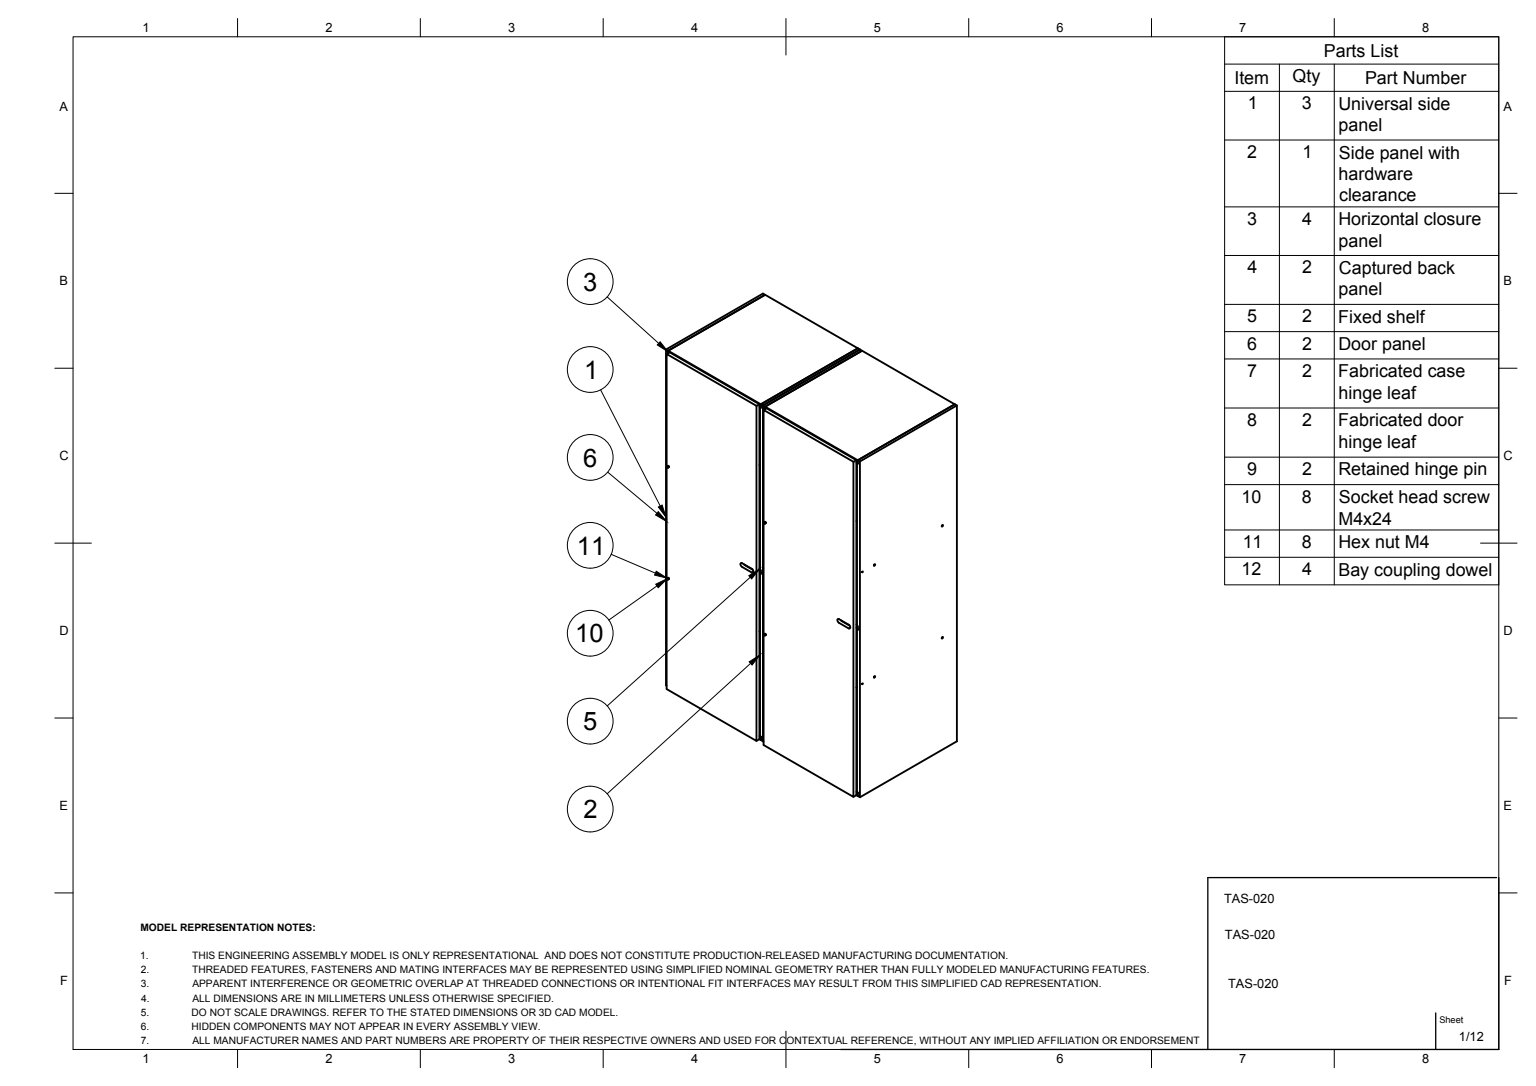
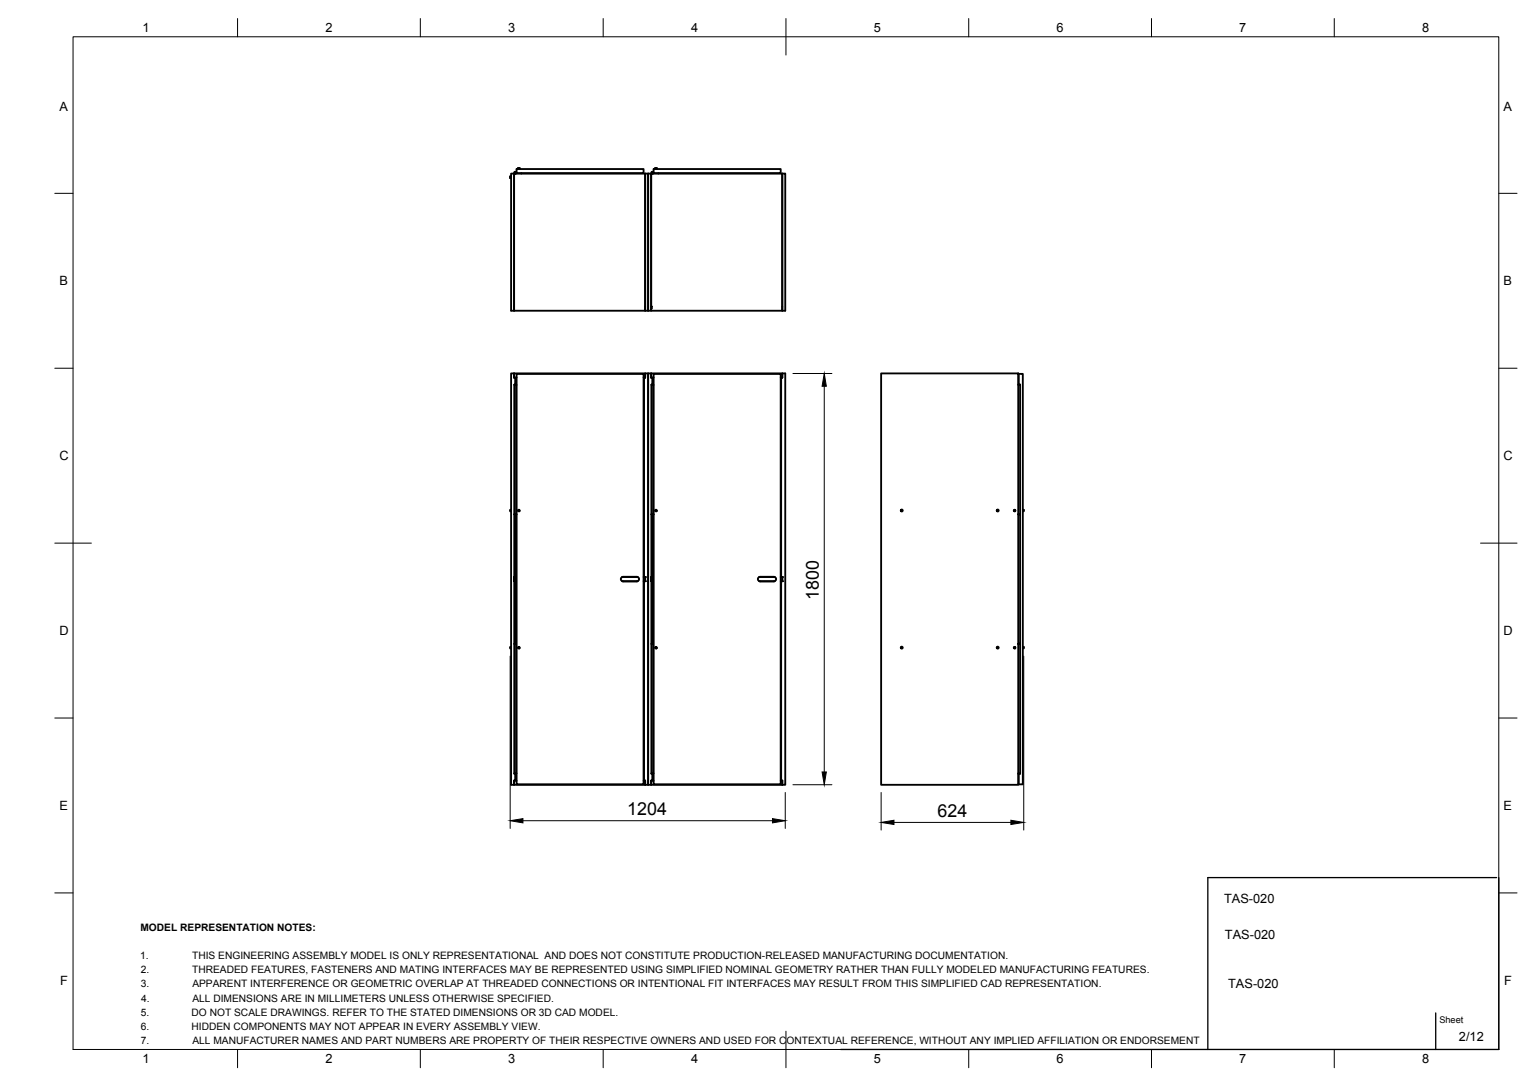
ISO-10303-21;
HEADER;
/* Generated by software containing ST-Developer
 * from STEP Tools, Inc. (www.steptools.com) 
 */

FILE_DESCRIPTION(
/* description */ (''),
/* implementation_level */ '2;1');

FILE_NAME(
/* name */ 'TAS-020.step',
/* time_stamp */ '2026-11-15T17:46:57-08:00',
/* author */ (''),
/* organization */ (''),
/* preprocessor_version */ 'ST-DEVELOPER v20.2',
/* originating_system */ 'Autodesk Translation Framework v15.17.0.0',
/* authorisation */ '');

FILE_SCHEMA (('AUTOMOTIVE_DESIGN { 1 0 10303 214 3 1 1 }'));
ENDSEC;

DATA;
#10=MECHANICAL_DESIGN_GEOMETRIC_PRESENTATION_REPRESENTATION('',(#375,#376,
#377,#378,#379,#380,#381,#382,#383,#384,#385,#386),#12963);
#11=ITEM_DEFINED_TRANSFORMATION($,$,#5008,#5301);
#12=ITEM_DEFINED_TRANSFORMATION($,$,#4955,#5302);
#13=ITEM_DEFINED_TRANSFORMATION($,$,#5053,#5303);
#14=ITEM_DEFINED_TRANSFORMATION($,$,#5064,#5304);
#15=ITEM_DEFINED_TRANSFORMATION($,$,#5071,#5305);
#16=ITEM_DEFINED_TRANSFORMATION($,$,#5080,#5306);
#17=ITEM_DEFINED_TRANSFORMATION($,$,#5101,#5307);
#18=ITEM_DEFINED_TRANSFORMATION($,$,#5134,#5308);
#19=ITEM_DEFINED_TRANSFORMATION($,$,#5163,#5309);
#20=ITEM_DEFINED_TRANSFORMATION($,$,#5177,#5310);
#21=ITEM_DEFINED_TRANSFORMATION($,$,#5267,#5311);
#22=ITEM_DEFINED_TRANSFORMATION($,$,#5295,#5312);
#23=ITEM_DEFINED_TRANSFORMATION($,$,#5053,#5313);
#24=ITEM_DEFINED_TRANSFORMATION($,$,#5177,#5314);
#25=ITEM_DEFINED_TRANSFORMATION($,$,#5267,#5315);
#26=ITEM_DEFINED_TRANSFORMATION($,$,#5177,#5316);
#27=ITEM_DEFINED_TRANSFORMATION($,$,#5267,#5317);
#28=ITEM_DEFINED_TRANSFORMATION($,$,#5177,#5318);
#29=ITEM_DEFINED_TRANSFORMATION($,$,#5267,#5319);
#30=ITEM_DEFINED_TRANSFORMATION($,$,#5008,#5320);
#31=ITEM_DEFINED_TRANSFORMATION($,$,#5008,#5321);
#32=ITEM_DEFINED_TRANSFORMATION($,$,#5053,#5322);
#33=ITEM_DEFINED_TRANSFORMATION($,$,#5053,#5323);
#34=ITEM_DEFINED_TRANSFORMATION($,$,#5064,#5324);
#35=ITEM_DEFINED_TRANSFORMATION($,$,#5071,#5325);
#36=ITEM_DEFINED_TRANSFORMATION($,$,#5080,#5326);
#37=ITEM_DEFINED_TRANSFORMATION($,$,#5101,#5327);
#38=ITEM_DEFINED_TRANSFORMATION($,$,#5134,#5328);
#39=ITEM_DEFINED_TRANSFORMATION($,$,#5163,#5329);
#40=ITEM_DEFINED_TRANSFORMATION($,$,#5177,#5330);
#41=ITEM_DEFINED_TRANSFORMATION($,$,#5267,#5331);
#42=ITEM_DEFINED_TRANSFORMATION($,$,#5177,#5332);
#43=ITEM_DEFINED_TRANSFORMATION($,$,#5267,#5333);
#44=ITEM_DEFINED_TRANSFORMATION($,$,#5177,#5334);
#45=ITEM_DEFINED_TRANSFORMATION($,$,#5267,#5335);
#46=ITEM_DEFINED_TRANSFORMATION($,$,#5177,#5336);
#47=ITEM_DEFINED_TRANSFORMATION($,$,#5267,#5337);
#48=ITEM_DEFINED_TRANSFORMATION($,$,#5295,#5338);
#49=ITEM_DEFINED_TRANSFORMATION($,$,#5295,#5339);
#50=ITEM_DEFINED_TRANSFORMATION($,$,#5295,#5340);
#51=(
REPRESENTATION_RELATIONSHIP($,$,#13036,#13034)
REPRESENTATION_RELATIONSHIP_WITH_TRANSFORMATION(#11)
SHAPE_REPRESENTATION_RELATIONSHIP()
);
#52=(
REPRESENTATION_RELATIONSHIP($,$,#13035,#13034)
REPRESENTATION_RELATIONSHIP_WITH_TRANSFORMATION(#12)
SHAPE_REPRESENTATION_RELATIONSHIP()
);
#53=(
REPRESENTATION_RELATIONSHIP($,$,#13037,#13034)
REPRESENTATION_RELATIONSHIP_WITH_TRANSFORMATION(#13)
SHAPE_REPRESENTATION_RELATIONSHIP()
);
#54=(
REPRESENTATION_RELATIONSHIP($,$,#13038,#13034)
REPRESENTATION_RELATIONSHIP_WITH_TRANSFORMATION(#14)
SHAPE_REPRESENTATION_RELATIONSHIP()
);
#55=(
REPRESENTATION_RELATIONSHIP($,$,#13039,#13034)
REPRESENTATION_RELATIONSHIP_WITH_TRANSFORMATION(#15)
SHAPE_REPRESENTATION_RELATIONSHIP()
);
#56=(
REPRESENTATION_RELATIONSHIP($,$,#13040,#13034)
REPRESENTATION_RELATIONSHIP_WITH_TRANSFORMATION(#16)
SHAPE_REPRESENTATION_RELATIONSHIP()
);
#57=(
REPRESENTATION_RELATIONSHIP($,$,#13041,#13034)
REPRESENTATION_RELATIONSHIP_WITH_TRANSFORMATION(#17)
SHAPE_REPRESENTATION_RELATIONSHIP()
);
#58=(
REPRESENTATION_RELATIONSHIP($,$,#13042,#13034)
REPRESENTATION_RELATIONSHIP_WITH_TRANSFORMATION(#18)
SHAPE_REPRESENTATION_RELATIONSHIP()
);
#59=(
REPRESENTATION_RELATIONSHIP($,$,#13043,#13034)
REPRESENTATION_RELATIONSHIP_WITH_TRANSFORMATION(#19)
SHAPE_REPRESENTATION_RELATIONSHIP()
);
#60=(
REPRESENTATION_RELATIONSHIP($,$,#13044,#13034)
REPRESENTATION_RELATIONSHIP_WITH_TRANSFORMATION(#20)
SHAPE_REPRESENTATION_RELATIONSHIP()
);
#61=(
REPRESENTATION_RELATIONSHIP($,$,#13045,#13034)
REPRESENTATION_RELATIONSHIP_WITH_TRANSFORMATION(#21)
SHAPE_REPRESENTATION_RELATIONSHIP()
);
#62=(
REPRESENTATION_RELATIONSHIP($,$,#13046,#13034)
REPRESENTATION_RELATIONSHIP_WITH_TRANSFORMATION(#22)
SHAPE_REPRESENTATION_RELATIONSHIP()
);
#63=(
REPRESENTATION_RELATIONSHIP($,$,#13037,#13034)
REPRESENTATION_RELATIONSHIP_WITH_TRANSFORMATION(#23)
SHAPE_REPRESENTATION_RELATIONSHIP()
);
#64=(
REPRESENTATION_RELATIONSHIP($,$,#13044,#13034)
REPRESENTATION_RELATIONSHIP_WITH_TRANSFORMATION(#24)
SHAPE_REPRESENTATION_RELATIONSHIP()
);
#65=(
REPRESENTATION_RELATIONSHIP($,$,#13045,#13034)
REPRESENTATION_RELATIONSHIP_WITH_TRANSFORMATION(#25)
SHAPE_REPRESENTATION_RELATIONSHIP()
);
#66=(
REPRESENTATION_RELATIONSHIP($,$,#13044,#13034)
REPRESENTATION_RELATIONSHIP_WITH_TRANSFORMATION(#26)
SHAPE_REPRESENTATION_RELATIONSHIP()
);
#67=(
REPRESENTATION_RELATIONSHIP($,$,#13045,#13034)
REPRESENTATION_RELATIONSHIP_WITH_TRANSFORMATION(#27)
SHAPE_REPRESENTATION_RELATIONSHIP()
);
#68=(
REPRESENTATION_RELATIONSHIP($,$,#13044,#13034)
REPRESENTATION_RELATIONSHIP_WITH_TRANSFORMATION(#28)
SHAPE_REPRESENTATION_RELATIONSHIP()
);
#69=(
REPRESENTATION_RELATIONSHIP($,$,#13045,#13034)
REPRESENTATION_RELATIONSHIP_WITH_TRANSFORMATION(#29)
SHAPE_REPRESENTATION_RELATIONSHIP()
);
#70=(
REPRESENTATION_RELATIONSHIP($,$,#13036,#13034)
REPRESENTATION_RELATIONSHIP_WITH_TRANSFORMATION(#30)
SHAPE_REPRESENTATION_RELATIONSHIP()
);
#71=(
REPRESENTATION_RELATIONSHIP($,$,#13036,#13034)
REPRESENTATION_RELATIONSHIP_WITH_TRANSFORMATION(#31)
SHAPE_REPRESENTATION_RELATIONSHIP()
);
#72=(
REPRESENTATION_RELATIONSHIP($,$,#13037,#13034)
REPRESENTATION_RELATIONSHIP_WITH_TRANSFORMATION(#32)
SHAPE_REPRESENTATION_RELATIONSHIP()
);
#73=(
REPRESENTATION_RELATIONSHIP($,$,#13037,#13034)
REPRESENTATION_RELATIONSHIP_WITH_TRANSFORMATION(#33)
SHAPE_REPRESENTATION_RELATIONSHIP()
);
#74=(
REPRESENTATION_RELATIONSHIP($,$,#13038,#13034)
REPRESENTATION_RELATIONSHIP_WITH_TRANSFORMATION(#34)
SHAPE_REPRESENTATION_RELATIONSHIP()
);
#75=(
REPRESENTATION_RELATIONSHIP($,$,#13039,#13034)
REPRESENTATION_RELATIONSHIP_WITH_TRANSFORMATION(#35)
SHAPE_REPRESENTATION_RELATIONSHIP()
);
#76=(
REPRESENTATION_RELATIONSHIP($,$,#13040,#13034)
REPRESENTATION_RELATIONSHIP_WITH_TRANSFORMATION(#36)
SHAPE_REPRESENTATION_RELATIONSHIP()
);
#77=(
REPRESENTATION_RELATIONSHIP($,$,#13041,#13034)
REPRESENTATION_RELATIONSHIP_WITH_TRANSFORMATION(#37)
SHAPE_REPRESENTATION_RELATIONSHIP()
);
#78=(
REPRESENTATION_RELATIONSHIP($,$,#13042,#13034)
REPRESENTATION_RELATIONSHIP_WITH_TRANSFORMATION(#38)
SHAPE_REPRESENTATION_RELATIONSHIP()
);
#79=(
REPRESENTATION_RELATIONSHIP($,$,#13043,#13034)
REPRESENTATION_RELATIONSHIP_WITH_TRANSFORMATION(#39)
SHAPE_REPRESENTATION_RELATIONSHIP()
);
#80=(
REPRESENTATION_RELATIONSHIP($,$,#13044,#13034)
REPRESENTATION_RELATIONSHIP_WITH_TRANSFORMATION(#40)
SHAPE_REPRESENTATION_RELATIONSHIP()
);
#81=(
REPRESENTATION_RELATIONSHIP($,$,#13045,#13034)
REPRESENTATION_RELATIONSHIP_WITH_TRANSFORMATION(#41)
SHAPE_REPRESENTATION_RELATIONSHIP()
);
#82=(
REPRESENTATION_RELATIONSHIP($,$,#13044,#13034)
REPRESENTATION_RELATIONSHIP_WITH_TRANSFORMATION(#42)
SHAPE_REPRESENTATION_RELATIONSHIP()
);
#83=(
REPRESENTATION_RELATIONSHIP($,$,#13045,#13034)
REPRESENTATION_RELATIONSHIP_WITH_TRANSFORMATION(#43)
SHAPE_REPRESENTATION_RELATIONSHIP()
);
#84=(
REPRESENTATION_RELATIONSHIP($,$,#13044,#13034)
REPRESENTATION_RELATIONSHIP_WITH_TRANSFORMATION(#44)
SHAPE_REPRESENTATION_RELATIONSHIP()
);
#85=(
REPRESENTATION_RELATIONSHIP($,$,#13045,#13034)
REPRESENTATION_RELATIONSHIP_WITH_TRANSFORMATION(#45)
SHAPE_REPRESENTATION_RELATIONSHIP()
);
#86=(
REPRESENTATION_RELATIONSHIP($,$,#13044,#13034)
REPRESENTATION_RELATIONSHIP_WITH_TRANSFORMATION(#46)
SHAPE_REPRESENTATION_RELATIONSHIP()
);
#87=(
REPRESENTATION_RELATIONSHIP($,$,#13045,#13034)
REPRESENTATION_RELATIONSHIP_WITH_TRANSFORMATION(#47)
SHAPE_REPRESENTATION_RELATIONSHIP()
);
#88=(
REPRESENTATION_RELATIONSHIP($,$,#13046,#13034)
REPRESENTATION_RELATIONSHIP_WITH_TRANSFORMATION(#48)
SHAPE_REPRESENTATION_RELATIONSHIP()
);
#89=(
REPRESENTATION_RELATIONSHIP($,$,#13046,#13034)
REPRESENTATION_RELATIONSHIP_WITH_TRANSFORMATION(#49)
SHAPE_REPRESENTATION_RELATIONSHIP()
);
#90=(
REPRESENTATION_RELATIONSHIP($,$,#13046,#13034)
REPRESENTATION_RELATIONSHIP_WITH_TRANSFORMATION(#50)
SHAPE_REPRESENTATION_RELATIONSHIP()
);
#91=CONTEXT_DEPENDENT_SHAPE_REPRESENTATION(#51,#12994);
#92=CONTEXT_DEPENDENT_SHAPE_REPRESENTATION(#52,#12995);
#93=CONTEXT_DEPENDENT_SHAPE_REPRESENTATION(#53,#12996);
#94=CONTEXT_DEPENDENT_SHAPE_REPRESENTATION(#54,#12997);
#95=CONTEXT_DEPENDENT_SHAPE_REPRESENTATION(#55,#12998);
#96=CONTEXT_DEPENDENT_SHAPE_REPRESENTATION(#56,#12999);
#97=CONTEXT_DEPENDENT_SHAPE_REPRESENTATION(#57,#13000);
#98=CONTEXT_DEPENDENT_SHAPE_REPRESENTATION(#58,#13001);
#99=CONTEXT_DEPENDENT_SHAPE_REPRESENTATION(#59,#13002);
#100=CONTEXT_DEPENDENT_SHAPE_REPRESENTATION(#60,#13003);
#101=CONTEXT_DEPENDENT_SHAPE_REPRESENTATION(#61,#13004);
#102=CONTEXT_DEPENDENT_SHAPE_REPRESENTATION(#62,#13005);
#103=CONTEXT_DEPENDENT_SHAPE_REPRESENTATION(#63,#13006);
#104=CONTEXT_DEPENDENT_SHAPE_REPRESENTATION(#64,#13007);
#105=CONTEXT_DEPENDENT_SHAPE_REPRESENTATION(#65,#13008);
#106=CONTEXT_DEPENDENT_SHAPE_REPRESENTATION(#66,#13009);
#107=CONTEXT_DEPENDENT_SHAPE_REPRESENTATION(#67,#13010);
#108=CONTEXT_DEPENDENT_SHAPE_REPRESENTATION(#68,#13011);
#109=CONTEXT_DEPENDENT_SHAPE_REPRESENTATION(#69,#13012);
#110=CONTEXT_DEPENDENT_SHAPE_REPRESENTATION(#70,#13013);
#111=CONTEXT_DEPENDENT_SHAPE_REPRESENTATION(#71,#13014);
#112=CONTEXT_DEPENDENT_SHAPE_REPRESENTATION(#72,#13015);
#113=CONTEXT_DEPENDENT_SHAPE_REPRESENTATION(#73,#13016);
#114=CONTEXT_DEPENDENT_SHAPE_REPRESENTATION(#74,#13017);
#115=CONTEXT_DEPENDENT_SHAPE_REPRESENTATION(#75,#13018);
#116=CONTEXT_DEPENDENT_SHAPE_REPRESENTATION(#76,#13019);
#117=CONTEXT_DEPENDENT_SHAPE_REPRESENTATION(#77,#13020);
#118=CONTEXT_DEPENDENT_SHAPE_REPRESENTATION(#78,#13021);
#119=CONTEXT_DEPENDENT_SHAPE_REPRESENTATION(#79,#13022);
#120=CONTEXT_DEPENDENT_SHAPE_REPRESENTATION(#80,#13023);
#121=CONTEXT_DEPENDENT_SHAPE_REPRESENTATION(#81,#13024);
#122=CONTEXT_DEPENDENT_SHAPE_REPRESENTATION(#82,#13025);
#123=CONTEXT_DEPENDENT_SHAPE_REPRESENTATION(#83,#13026);
#124=CONTEXT_DEPENDENT_SHAPE_REPRESENTATION(#84,#13027);
#125=CONTEXT_DEPENDENT_SHAPE_REPRESENTATION(#85,#13028);
#126=CONTEXT_DEPENDENT_SHAPE_REPRESENTATION(#86,#13029);
#127=CONTEXT_DEPENDENT_SHAPE_REPRESENTATION(#87,#13030);
#128=CONTEXT_DEPENDENT_SHAPE_REPRESENTATION(#88,#13031);
#129=CONTEXT_DEPENDENT_SHAPE_REPRESENTATION(#89,#13032);
#130=CONTEXT_DEPENDENT_SHAPE_REPRESENTATION(#90,#13033);
#131=NEXT_ASSEMBLY_USAGE_OCCURRENCE('Universal side panel:1',
'Universal side panel:1','Universal side panel:1',#13048,#13050,
'Universal side panel:1');
#132=NEXT_ASSEMBLY_USAGE_OCCURRENCE(
'Side panel with hardware clearance:1',
'Side panel with hardware clearance:1',
'Side panel with hardware clearance:1',#13048,#13049,
'Side panel with hardware clearance:1');
#133=NEXT_ASSEMBLY_USAGE_OCCURRENCE('Horizontal closure panel:1',
'Horizontal closure panel:1','Horizontal closure panel:1',#13048,#13051,
'Horizontal closure panel:1');
#134=NEXT_ASSEMBLY_USAGE_OCCURRENCE('Captured back panel:1',
'Captured back panel:1','Captured back panel:1',#13048,#13052,
'Captured back panel:1');
#135=NEXT_ASSEMBLY_USAGE_OCCURRENCE('Fixed shelf:1','Fixed shelf:1',
'Fixed shelf:1',#13048,#13053,'Fixed shelf:1');
#136=NEXT_ASSEMBLY_USAGE_OCCURRENCE('Door panel:1','Door panel:1',
'Door panel:1',#13048,#13054,'Door panel:1');
#137=NEXT_ASSEMBLY_USAGE_OCCURRENCE('Fabricated case hinge leaf:1',
'Fabricated case hinge leaf:1','Fabricated case hinge leaf:1',#13048,#13055,
'Fabricated case hinge leaf:1');
#138=NEXT_ASSEMBLY_USAGE_OCCURRENCE('Fabricated door hinge leaf:1',
'Fabricated door hinge leaf:1','Fabricated door hinge leaf:1',#13048,#13056,
'Fabricated door hinge leaf:1');
#139=NEXT_ASSEMBLY_USAGE_OCCURRENCE('Retained hinge pin:1',
'Retained hinge pin:1','Retained hinge pin:1',#13048,#13057,
'Retained hinge pin:1');
#140=NEXT_ASSEMBLY_USAGE_OCCURRENCE('Socket head screw M4x24:1',
'Socket head screw M4x24:1','Socket head screw M4x24:1',#13048,#13058,
'Socket head screw M4x24:1');
#141=NEXT_ASSEMBLY_USAGE_OCCURRENCE('Hex nut M4:1','Hex nut M4:1',
'Hex nut M4:1',#13048,#13059,'Hex nut M4:1');
#142=NEXT_ASSEMBLY_USAGE_OCCURRENCE('Bay coupling dowel:1',
'Bay coupling dowel:1','Bay coupling dowel:1',#13048,#13060,
'Bay coupling dowel:1');
#143=NEXT_ASSEMBLY_USAGE_OCCURRENCE('Horizontal closure panel:2',
'Horizontal closure panel:2','Horizontal closure panel:2',#13048,#13051,
'Horizontal closure panel:2');
#144=NEXT_ASSEMBLY_USAGE_OCCURRENCE('Socket head screw M4x24:2',
'Socket head screw M4x24:2','Socket head screw M4x24:2',#13048,#13058,
'Socket head screw M4x24:2');
#145=NEXT_ASSEMBLY_USAGE_OCCURRENCE('Hex nut M4:2','Hex nut M4:2',
'Hex nut M4:2',#13048,#13059,'Hex nut M4:2');
#146=NEXT_ASSEMBLY_USAGE_OCCURRENCE('Socket head screw M4x24:3',
'Socket head screw M4x24:3','Socket head screw M4x24:3',#13048,#13058,
'Socket head screw M4x24:3');
#147=NEXT_ASSEMBLY_USAGE_OCCURRENCE('Hex nut M4:3','Hex nut M4:3',
'Hex nut M4:3',#13048,#13059,'Hex nut M4:3');
#148=NEXT_ASSEMBLY_USAGE_OCCURRENCE('Socket head screw M4x24:4',
'Socket head screw M4x24:4','Socket head screw M4x24:4',#13048,#13058,
'Socket head screw M4x24:4');
#149=NEXT_ASSEMBLY_USAGE_OCCURRENCE('Hex nut M4:4','Hex nut M4:4',
'Hex nut M4:4',#13048,#13059,'Hex nut M4:4');
#150=NEXT_ASSEMBLY_USAGE_OCCURRENCE('Universal side panel:2',
'Universal side panel:2','Universal side panel:2',#13048,#13050,
'Universal side panel:2');
#151=NEXT_ASSEMBLY_USAGE_OCCURRENCE('Universal side panel:3',
'Universal side panel:3','Universal side panel:3',#13048,#13050,
'Universal side panel:3');
#152=NEXT_ASSEMBLY_USAGE_OCCURRENCE('Horizontal closure panel:3',
'Horizontal closure panel:3','Horizontal closure panel:3',#13048,#13051,
'Horizontal closure panel:3');
#153=NEXT_ASSEMBLY_USAGE_OCCURRENCE('Horizontal closure panel:4',
'Horizontal closure panel:4','Horizontal closure panel:4',#13048,#13051,
'Horizontal closure panel:4');
#154=NEXT_ASSEMBLY_USAGE_OCCURRENCE('Captured back panel:2',
'Captured back panel:2','Captured back panel:2',#13048,#13052,
'Captured back panel:2');
#155=NEXT_ASSEMBLY_USAGE_OCCURRENCE('Fixed shelf:2','Fixed shelf:2',
'Fixed shelf:2',#13048,#13053,'Fixed shelf:2');
#156=NEXT_ASSEMBLY_USAGE_OCCURRENCE('Door panel:2','Door panel:2',
'Door panel:2',#13048,#13054,'Door panel:2');
#157=NEXT_ASSEMBLY_USAGE_OCCURRENCE('Fabricated case hinge leaf:2',
'Fabricated case hinge leaf:2','Fabricated case hinge leaf:2',#13048,#13055,
'Fabricated case hinge leaf:2');
#158=NEXT_ASSEMBLY_USAGE_OCCURRENCE('Fabricated door hinge leaf:2',
'Fabricated door hinge leaf:2','Fabricated door hinge leaf:2',#13048,#13056,
'Fabricated door hinge leaf:2');
#159=NEXT_ASSEMBLY_USAGE_OCCURRENCE('Retained hinge pin:2',
'Retained hinge pin:2','Retained hinge pin:2',#13048,#13057,
'Retained hinge pin:2');
#160=NEXT_ASSEMBLY_USAGE_OCCURRENCE('Socket head screw M4x24:5',
'Socket head screw M4x24:5','Socket head screw M4x24:5',#13048,#13058,
'Socket head screw M4x24:5');
#161=NEXT_ASSEMBLY_USAGE_OCCURRENCE('Hex nut M4:5','Hex nut M4:5',
'Hex nut M4:5',#13048,#13059,'Hex nut M4:5');
#162=NEXT_ASSEMBLY_USAGE_OCCURRENCE('Socket head screw M4x24:6',
'Socket head screw M4x24:6','Socket head screw M4x24:6',#13048,#13058,
'Socket head screw M4x24:6');
#163=NEXT_ASSEMBLY_USAGE_OCCURRENCE('Hex nut M4:6','Hex nut M4:6',
'Hex nut M4:6',#13048,#13059,'Hex nut M4:6');
#164=NEXT_ASSEMBLY_USAGE_OCCURRENCE('Socket head screw M4x24:7',
'Socket head screw M4x24:7','Socket head screw M4x24:7',#13048,#13058,
'Socket head screw M4x24:7');
#165=NEXT_ASSEMBLY_USAGE_OCCURRENCE('Hex nut M4:7','Hex nut M4:7',
'Hex nut M4:7',#13048,#13059,'Hex nut M4:7');
#166=NEXT_ASSEMBLY_USAGE_OCCURRENCE('Socket head screw M4x24:8',
'Socket head screw M4x24:8','Socket head screw M4x24:8',#13048,#13058,
'Socket head screw M4x24:8');
#167=NEXT_ASSEMBLY_USAGE_OCCURRENCE('Hex nut M4:8','Hex nut M4:8',
'Hex nut M4:8',#13048,#13059,'Hex nut M4:8');
#168=NEXT_ASSEMBLY_USAGE_OCCURRENCE('Bay coupling dowel:2',
'Bay coupling dowel:2','Bay coupling dowel:2',#13048,#13060,
'Bay coupling dowel:2');
#169=NEXT_ASSEMBLY_USAGE_OCCURRENCE('Bay coupling dowel:3',
'Bay coupling dowel:3','Bay coupling dowel:3',#13048,#13060,
'Bay coupling dowel:3');
#170=NEXT_ASSEMBLY_USAGE_OCCURRENCE('Bay coupling dowel:4',
'Bay coupling dowel:4','Bay coupling dowel:4',#13048,#13060,
'Bay coupling dowel:4');
#171=B_SPLINE_SURFACE_WITH_KNOTS('',3,3,((#9802,#9803,#9804,#9805,#9806,
#9807,#9808,#9809,#9810,#9811,#9812,#9813,#9814,#9815,#9816,#9817,#9818,
#9819,#9820,#9821,#9822,#9823,#9824,#9825,#9826,#9827,#9828,#9829,#9830,
#9831,#9832,#9833,#9834,#9835,#9836,#9837,#9838,#9839,#9840,#9841,#9842,
#9843,#9844,#9845,#9846,#9847,#9848,#9849,#9850,#9851,#9852,#9853,#9854,
#9855,#9856,#9857,#9858,#9859,#9860,#9861,#9862,#9863,#9864,#9865,#9866,
#9867,#9868,#9869,#9870,#9871,#9872,#9873,#9874,#9875,#9876,#9877,#9878,
#9879,#9880,#9881,#9882,#9883,#9884,#9885,#9886,#9887,#9888,#9889,#9890,
#9891,#9892,#9893,#9894,#9895,#9896,#9897,#9898,#9899,#9900,#9901,#9902,
#9903,#9904,#9905,#9906,#9907,#9908,#9909,#9910,#9911,#9912,#9913,#9914,
#9915,#9916,#9917,#9918,#9919,#9920,#9921,#9922,#9923,#9924,#9925,#9926,
#9927,#9928,#9929,#9930,#9931,#9932,#9933,#9934,#9935,#9936,#9937,#9938,
#9939,#9940,#9941,#9942,#9943,#9944,#9945,#9946,#9947,#9948,#9949,#9950,
#9951,#9952,#9953,#9954,#9955,#9956,#9957,#9958,#9959,#9960,#9961,#9962,
#9963,#9964,#9965,#9966,#9967,#9968,#9969,#9970,#9971,#9972,#9973,#9974,
#9975,#9976,#9977,#9978,#9979,#9980,#9981,#9982,#9983,#9984,#9985,#9986,
#9987,#9988,#9989,#9990,#9991,#9992,#9993,#9994,#9995,#9996,#9997,#9998,
#9999,#10000,#10001,#10002,#10003,#10004,#10005,#10006,#10007,#10008,#10009,
#10010,#10011,#10012,#10013,#10014,#10015,#10016,#10017,#10018,#10019,#10020,
#10021,#10022),(#10023,#10024,#10025,#10026,#10027,#10028,#10029,#10030,
#10031,#10032,#10033,#10034,#10035,#10036,#10037,#10038,#10039,#10040,#10041,
#10042,#10043,#10044,#10045,#10046,#10047,#10048,#10049,#10050,#10051,#10052,
#10053,#10054,#10055,#10056,#10057,#10058,#10059,#10060,#10061,#10062,#10063,
#10064,#10065,#10066,#10067,#10068,#10069,#10070,#10071,#10072,#10073,#10074,
#10075,#10076,#10077,#10078,#10079,#10080,#10081,#10082,#10083,#10084,#10085,
#10086,#10087,#10088,#10089,#10090,#10091,#10092,#10093,#10094,#10095,#10096,
#10097,#10098,#10099,#10100,#10101,#10102,#10103,#10104,#10105,#10106,#10107,
#10108,#10109,#10110,#10111,#10112,#10113,#10114,#10115,#10116,#10117,#10118,
#10119,#10120,#10121,#10122,#10123,#10124,#10125,#10126,#10127,#10128,#10129,
#10130,#10131,#10132,#10133,#10134,#10135,#10136,#10137,#10138,#10139,#10140,
#10141,#10142,#10143,#10144,#10145,#10146,#10147,#10148,#10149,#10150,#10151,
#10152,#10153,#10154,#10155,#10156,#10157,#10158,#10159,#10160,#10161,#10162,
#10163,#10164,#10165,#10166,#10167,#10168,#10169,#10170,#10171,#10172,#10173,
#10174,#10175,#10176,#10177,#10178,#10179,#10180,#10181,#10182,#10183,#10184,
#10185,#10186,#10187,#10188,#10189,#10190,#10191,#10192,#10193,#10194,#10195,
#10196,#10197,#10198,#10199,#10200,#10201,#10202,#10203,#10204,#10205,#10206,
#10207,#10208,#10209,#10210,#10211,#10212,#10213,#10214,#10215,#10216,#10217,
#10218,#10219,#10220,#10221,#10222,#10223,#10224,#10225,#10226,#10227,#10228,
#10229,#10230,#10231,#10232,#10233,#10234,#10235,#10236,#10237,#10238,#10239,
#10240,#10241,#10242,#10243),(#10244,#10245,#10246,#10247,#10248,#10249,
#10250,#10251,#10252,#10253,#10254,#10255,#10256,#10257,#10258,#10259,#10260,
#10261,#10262,#10263,#10264,#10265,#10266,#10267,#10268,#10269,#10270,#10271,
#10272,#10273,#10274,#10275,#10276,#10277,#10278,#10279,#10280,#10281,#10282,
#10283,#10284,#10285,#10286,#10287,#10288,#10289,#10290,#10291,#10292,#10293,
#10294,#10295,#10296,#10297,#10298,#10299,#10300,#10301,#10302,#10303,#10304,
#10305,#10306,#10307,#10308,#10309,#10310,#10311,#10312,#10313,#10314,#10315,
#10316,#10317,#10318,#10319,#10320,#10321,#10322,#10323,#10324,#10325,#10326,
#10327,#10328,#10329,#10330,#10331,#10332,#10333,#10334,#10335,#10336,#10337,
#10338,#10339,#10340,#10341,#10342,#10343,#10344,#10345,#10346,#10347,#10348,
#10349,#10350,#10351,#10352,#10353,#10354,#10355,#10356,#10357,#10358,#10359,
#10360,#10361,#10362,#10363,#10364,#10365,#10366,#10367,#10368,#10369,#10370,
#10371,#10372,#10373,#10374,#10375,#10376,#10377,#10378,#10379,#10380,#10381,
#10382,#10383,#10384,#10385,#10386,#10387,#10388,#10389,#10390,#10391,#10392,
#10393,#10394,#10395,#10396,#10397,#10398,#10399,#10400,#10401,#10402,#10403,
#10404,#10405,#10406,#10407,#10408,#10409,#10410,#10411,#10412,#10413,#10414,
#10415,#10416,#10417,#10418,#10419,#10420,#10421,#10422,#10423,#10424,#10425,
#10426,#10427,#10428,#10429,#10430,#10431,#10432,#10433,#10434,#10435,#10436,
#10437,#10438,#10439,#10440,#10441,#10442,#10443,#10444,#10445,#10446,#10447,
#10448,#10449,#10450,#10451,#10452,#10453,#10454,#10455,#10456,#10457,#10458,
#10459,#10460,#10461,#10462,#10463,#10464),(#10465,#10466,#10467,#10468,
#10469,#10470,#10471,#10472,#10473,#10474,#10475,#10476,#10477,#10478,#10479,
#10480,#10481,#10482,#10483,#10484,#10485,#10486,#10487,#10488,#10489,#10490,
#10491,#10492,#10493,#10494,#10495,#10496,#10497,#10498,#10499,#10500,#10501,
#10502,#10503,#10504,#10505,#10506,#10507,#10508,#10509,#10510,#10511,#10512,
#10513,#10514,#10515,#10516,#10517,#10518,#10519,#10520,#10521,#10522,#10523,
#10524,#10525,#10526,#10527,#10528,#10529,#10530,#10531,#10532,#10533,#10534,
#10535,#10536,#10537,#10538,#10539,#10540,#10541,#10542,#10543,#10544,#10545,
#10546,#10547,#10548,#10549,#10550,#10551,#10552,#10553,#10554,#10555,#10556,
#10557,#10558,#10559,#10560,#10561,#10562,#10563,#10564,#10565,#10566,#10567,
#10568,#10569,#10570,#10571,#10572,#10573,#10574,#10575,#10576,#10577,#10578,
#10579,#10580,#10581,#10582,#10583,#10584,#10585,#10586,#10587,#10588,#10589,
#10590,#10591,#10592,#10593,#10594,#10595,#10596,#10597,#10598,#10599,#10600,
#10601,#10602,#10603,#10604,#10605,#10606,#10607,#10608,#10609,#10610,#10611,
#10612,#10613,#10614,#10615,#10616,#10617,#10618,#10619,#10620,#10621,#10622,
#10623,#10624,#10625,#10626,#10627,#10628,#10629,#10630,#10631,#10632,#10633,
#10634,#10635,#10636,#10637,#10638,#10639,#10640,#10641,#10642,#10643,#10644,
#10645,#10646,#10647,#10648,#10649,#10650,#10651,#10652,#10653,#10654,#10655,
#10656,#10657,#10658,#10659,#10660,#10661,#10662,#10663,#10664,#10665,#10666,
#10667,#10668,#10669,#10670,#10671,#10672,#10673,#10674,#10675,#10676,#10677,
#10678,#10679,#10680,#10681,#10682,#10683,#10684,#10685)),.UNSPECIFIED.,
 .F.,.F.,.F.,(4,4),(4,1,1,1,1,1,1,1,1,1,1,1,1,1,1,1,1,1,1,1,1,1,1,1,1,1,
1,1,1,1,1,1,1,1,1,1,1,1,1,1,1,1,1,1,1,1,1,1,1,1,1,1,1,1,1,1,1,1,1,1,1,1,
1,1,1,1,1,1,1,1,1,1,1,1,1,1,1,1,1,1,1,1,1,1,1,1,1,1,1,1,1,1,1,1,1,1,1,1,
1,1,1,1,1,1,1,1,1,1,1,1,1,1,1,1,1,1,1,1,1,1,1,1,1,1,1,1,1,1,1,1,1,1,1,1,
1,1,1,1,1,1,1,1,1,1,1,1,1,1,1,1,1,1,1,1,1,1,1,1,1,1,1,1,1,1,1,1,1,1,1,1,
1,1,1,1,1,1,1,1,1,1,1,1,1,1,1,1,1,1,1,1,1,1,1,1,1,1,1,1,1,1,1,1,1,1,1,1,
1,1,1,1,1,1,1,1,1,1,1,1,4),(0.,0.0460148164544132),(8.31058692273996,9.30824121805847,
10.305895513377,11.3035498086955,12.301204104014,13.2988583993325,14.296512694651,
15.2941669899695,16.291821285288,17.2894755806066,18.2871298759251,19.2847841712436,
20.2824384665621,21.2800927618806,22.2777470571991,23.2754013525176,24.2730556478361,
25.2707099431546,26.2683642384732,27.2660185337917,28.2636728291102,29.2613271244287,
30.2589814197472,31.2566357150657,32.2542900103842,33.2519443057027,34.2495986010213,
35.2472528963398,36.2449071916583,37.2425614869768,38.2402157822953,39.2378700776138,
40.2355243729323,41.2331786682508,42.2308329635693,43.2284872588879,44.2261415542064,
45.2237958495249,46.2214501448434,47.2191044401619,48.2167587354804,49.2144130307989,
50.2120673261174,51.209721621436,52.2073759167545,53.205030212073,54.2026845073915,
55.20033880271,56.1979930980285,57.195647393347,58.1933016886655,59.190955983984,
60.1886102793026,61.1862645746211,62.1839188699396,63.1815731652581,64.1792274605766,
65.1768817558951,66.1745360512136,67.1721903465321,68.1698446418506,69.1674989371692,
70.1651532324877,71.1628075278062,72.1604618231247,73.1581161184432,74.1557704137617,
75.1534247090802,76.1510790043987,77.1487332997173,78.1463875950358,79.1440418903543,
80.1416961856728,81.1393504809913,82.1370047763098,83.1346590716283,84.1323133669468,
85.1299676622653,86.1276219575839,87.1252762529024,88.1229305482209,89.1205848435394,
90.1182391388579,91.1158934341764,92.1135477294949,93.1112020248134,94.1088563201319,
95.1065106154505,96.104164910769,97.1018192060875,98.099473501406,99.0971277967245,
100.094782092043,101.092436387362,102.09009068268,103.087744977999,104.085399273317,
105.083053568636,106.080707863954,107.078362159273,108.076016454591,109.07367074991,
110.071325045228,111.068979340547,112.066633635865,113.064287931184,114.061942226502,
115.059596521821,116.057250817139,117.054905112458,118.052559407776,119.050213703095,
120.047867998413,121.045522293732,122.04317658905,123.040830884369,124.038485179687,
125.036139475006,126.033793770324,127.031448065643,128.029102360961,129.02675665628,
130.024410951598,131.022065246917,132.019719542235,133.017373837554,134.015028132872,
135.012682428191,136.010336723509,137.007991018828,138.005645314146,139.003299609465,
140.000953904783,140.998608200102,141.99626249542,142.993916790739,143.991571086058,
144.989225381376,145.986879676695,146.984533972013,147.982188267332,148.97984256265,
149.977496857969,150.975151153287,151.972805448606,152.970459743924,153.968114039243,
154.965768334561,155.96342262988,156.961076925198,157.958731220517,158.956385515835,
159.954039811154,160.951694106472,161.949348401791,162.947002697109,163.944656992428,
164.942311287746,165.939965583065,166.937619878383,167.935274173702,168.93292846902,
169.930582764339,170.928237059657,171.925891354976,172.923545650294,173.921199945613,
174.918854240931,175.91650853625,176.914162831568,177.911817126887,178.909471422205,
179.907125717524,180.904780012842,181.902434308161,182.900088603479,183.897742898798,
184.895397194116,185.893051489435,186.890705784754,187.888360080072,188.886014375391,
189.883668670709,190.881322966028,191.878977261346,192.876631556665,193.874285851983,
194.871940147302,195.86959444262,196.867248737939,197.864903033257,198.862557328576,
199.860211623894,200.857865919213,201.855520214531,202.85317450985,203.850828805168,
204.848483100487,205.846137395805,206.843791691124,207.841445986442,208.839100281761,
209.836754577079,210.834408872398,211.832063167716,212.829717463035,213.827371758353,
214.825026053672,215.82268034899,216.820334644309,217.817988939627,218.815643234946,
219.813297530264,220.810951825583,221.808606120901,222.80626041622,223.803914711538,
224.801569006857,225.799223302175),.UNSPECIFIED.);
#172=B_SPLINE_SURFACE_WITH_KNOTS('',3,3,((#10819,#10820,#10821,#10822,#10823,
#10824,#10825,#10826,#10827,#10828,#10829,#10830,#10831,#10832,#10833,#10834,
#10835,#10836,#10837,#10838,#10839,#10840,#10841,#10842,#10843,#10844,#10845,
#10846,#10847,#10848,#10849,#10850,#10851,#10852,#10853,#10854,#10855,#10856,
#10857,#10858,#10859,#10860,#10861,#10862,#10863,#10864,#10865,#10866,#10867,
#10868,#10869,#10870,#10871,#10872,#10873,#10874,#10875,#10876,#10877,#10878,
#10879,#10880,#10881,#10882,#10883,#10884,#10885,#10886,#10887,#10888,#10889,
#10890,#10891,#10892,#10893,#10894,#10895,#10896,#10897,#10898,#10899,#10900,
#10901,#10902,#10903,#10904,#10905,#10906,#10907,#10908,#10909,#10910,#10911,
#10912,#10913,#10914,#10915,#10916,#10917,#10918,#10919,#10920,#10921,#10922,
#10923,#10924,#10925,#10926,#10927,#10928,#10929,#10930,#10931,#10932,#10933,
#10934,#10935,#10936,#10937,#10938,#10939,#10940,#10941,#10942,#10943,#10944,
#10945,#10946,#10947,#10948,#10949,#10950,#10951,#10952,#10953,#10954,#10955,
#10956,#10957,#10958,#10959,#10960,#10961,#10962,#10963,#10964,#10965,#10966,
#10967,#10968,#10969,#10970,#10971,#10972,#10973,#10974,#10975,#10976,#10977,
#10978,#10979,#10980,#10981,#10982,#10983,#10984,#10985,#10986,#10987,#10988,
#10989,#10990,#10991,#10992,#10993,#10994,#10995,#10996,#10997,#10998,#10999,
#11000,#11001,#11002,#11003,#11004,#11005,#11006,#11007,#11008,#11009,#11010,
#11011,#11012,#11013,#11014,#11015,#11016,#11017,#11018,#11019,#11020,#11021,
#11022,#11023,#11024,#11025,#11026,#11027,#11028,#11029,#11030,#11031,#11032,
#11033,#11034,#11035,#11036,#11037,#11038,#11039),(#11040,#11041,#11042,
#11043,#11044,#11045,#11046,#11047,#11048,#11049,#11050,#11051,#11052,#11053,
#11054,#11055,#11056,#11057,#11058,#11059,#11060,#11061,#11062,#11063,#11064,
#11065,#11066,#11067,#11068,#11069,#11070,#11071,#11072,#11073,#11074,#11075,
#11076,#11077,#11078,#11079,#11080,#11081,#11082,#11083,#11084,#11085,#11086,
#11087,#11088,#11089,#11090,#11091,#11092,#11093,#11094,#11095,#11096,#11097,
#11098,#11099,#11100,#11101,#11102,#11103,#11104,#11105,#11106,#11107,#11108,
#11109,#11110,#11111,#11112,#11113,#11114,#11115,#11116,#11117,#11118,#11119,
#11120,#11121,#11122,#11123,#11124,#11125,#11126,#11127,#11128,#11129,#11130,
#11131,#11132,#11133,#11134,#11135,#11136,#11137,#11138,#11139,#11140,#11141,
#11142,#11143,#11144,#11145,#11146,#11147,#11148,#11149,#11150,#11151,#11152,
#11153,#11154,#11155,#11156,#11157,#11158,#11159,#11160,#11161,#11162,#11163,
#11164,#11165,#11166,#11167,#11168,#11169,#11170,#11171,#11172,#11173,#11174,
#11175,#11176,#11177,#11178,#11179,#11180,#11181,#11182,#11183,#11184,#11185,
#11186,#11187,#11188,#11189,#11190,#11191,#11192,#11193,#11194,#11195,#11196,
#11197,#11198,#11199,#11200,#11201,#11202,#11203,#11204,#11205,#11206,#11207,
#11208,#11209,#11210,#11211,#11212,#11213,#11214,#11215,#11216,#11217,#11218,
#11219,#11220,#11221,#11222,#11223,#11224,#11225,#11226,#11227,#11228,#11229,
#11230,#11231,#11232,#11233,#11234,#11235,#11236,#11237,#11238,#11239,#11240,
#11241,#11242,#11243,#11244,#11245,#11246,#11247,#11248,#11249,#11250,#11251,
#11252,#11253,#11254,#11255,#11256,#11257,#11258,#11259,#11260),(#11261,
#11262,#11263,#11264,#11265,#11266,#11267,#11268,#11269,#11270,#11271,#11272,
#11273,#11274,#11275,#11276,#11277,#11278,#11279,#11280,#11281,#11282,#11283,
#11284,#11285,#11286,#11287,#11288,#11289,#11290,#11291,#11292,#11293,#11294,
#11295,#11296,#11297,#11298,#11299,#11300,#11301,#11302,#11303,#11304,#11305,
#11306,#11307,#11308,#11309,#11310,#11311,#11312,#11313,#11314,#11315,#11316,
#11317,#11318,#11319,#11320,#11321,#11322,#11323,#11324,#11325,#11326,#11327,
#11328,#11329,#11330,#11331,#11332,#11333,#11334,#11335,#11336,#11337,#11338,
#11339,#11340,#11341,#11342,#11343,#11344,#11345,#11346,#11347,#11348,#11349,
#11350,#11351,#11352,#11353,#11354,#11355,#11356,#11357,#11358,#11359,#11360,
#11361,#11362,#11363,#11364,#11365,#11366,#11367,#11368,#11369,#11370,#11371,
#11372,#11373,#11374,#11375,#11376,#11377,#11378,#11379,#11380,#11381,#11382,
#11383,#11384,#11385,#11386,#11387,#11388,#11389,#11390,#11391,#11392,#11393,
#11394,#11395,#11396,#11397,#11398,#11399,#11400,#11401,#11402,#11403,#11404,
#11405,#11406,#11407,#11408,#11409,#11410,#11411,#11412,#11413,#11414,#11415,
#11416,#11417,#11418,#11419,#11420,#11421,#11422,#11423,#11424,#11425,#11426,
#11427,#11428,#11429,#11430,#11431,#11432,#11433,#11434,#11435,#11436,#11437,
#11438,#11439,#11440,#11441,#11442,#11443,#11444,#11445,#11446,#11447,#11448,
#11449,#11450,#11451,#11452,#11453,#11454,#11455,#11456,#11457,#11458,#11459,
#11460,#11461,#11462,#11463,#11464,#11465,#11466,#11467,#11468,#11469,#11470,
#11471,#11472,#11473,#11474,#11475,#11476,#11477,#11478,#11479,#11480,#11481),
(#11482,#11483,#11484,#11485,#11486,#11487,#11488,#11489,#11490,#11491,
#11492,#11493,#11494,#11495,#11496,#11497,#11498,#11499,#11500,#11501,#11502,
#11503,#11504,#11505,#11506,#11507,#11508,#11509,#11510,#11511,#11512,#11513,
#11514,#11515,#11516,#11517,#11518,#11519,#11520,#11521,#11522,#11523,#11524,
#11525,#11526,#11527,#11528,#11529,#11530,#11531,#11532,#11533,#11534,#11535,
#11536,#11537,#11538,#11539,#11540,#11541,#11542,#11543,#11544,#11545,#11546,
#11547,#11548,#11549,#11550,#11551,#11552,#11553,#11554,#11555,#11556,#11557,
#11558,#11559,#11560,#11561,#11562,#11563,#11564,#11565,#11566,#11567,#11568,
#11569,#11570,#11571,#11572,#11573,#11574,#11575,#11576,#11577,#11578,#11579,
#11580,#11581,#11582,#11583,#11584,#11585,#11586,#11587,#11588,#11589,#11590,
#11591,#11592,#11593,#11594,#11595,#11596,#11597,#11598,#11599,#11600,#11601,
#11602,#11603,#11604,#11605,#11606,#11607,#11608,#11609,#11610,#11611,#11612,
#11613,#11614,#11615,#11616,#11617,#11618,#11619,#11620,#11621,#11622,#11623,
#11624,#11625,#11626,#11627,#11628,#11629,#11630,#11631,#11632,#11633,#11634,
#11635,#11636,#11637,#11638,#11639,#11640,#11641,#11642,#11643,#11644,#11645,
#11646,#11647,#11648,#11649,#11650,#11651,#11652,#11653,#11654,#11655,#11656,
#11657,#11658,#11659,#11660,#11661,#11662,#11663,#11664,#11665,#11666,#11667,
#11668,#11669,#11670,#11671,#11672,#11673,#11674,#11675,#11676,#11677,#11678,
#11679,#11680,#11681,#11682,#11683,#11684,#11685,#11686,#11687,#11688,#11689,
#11690,#11691,#11692,#11693,#11694,#11695,#11696,#11697,#11698,#11699,#11700,
#11701,#11702)),.UNSPECIFIED.,.F.,.F.,.F.,(4,4),(4,1,1,1,1,1,1,1,1,1,1,
1,1,1,1,1,1,1,1,1,1,1,1,1,1,1,1,1,1,1,1,1,1,1,1,1,1,1,1,1,1,1,1,1,1,1,1,
1,1,1,1,1,1,1,1,1,1,1,1,1,1,1,1,1,1,1,1,1,1,1,1,1,1,1,1,1,1,1,1,1,1,1,1,
1,1,1,1,1,1,1,1,1,1,1,1,1,1,1,1,1,1,1,1,1,1,1,1,1,1,1,1,1,1,1,1,1,1,1,1,
1,1,1,1,1,1,1,1,1,1,1,1,1,1,1,1,1,1,1,1,1,1,1,1,1,1,1,1,1,1,1,1,1,1,1,1,
1,1,1,1,1,1,1,1,1,1,1,1,1,1,1,1,1,1,1,1,1,1,1,1,1,1,1,1,1,1,1,1,1,1,1,1,
1,1,1,1,1,1,1,1,1,1,1,1,1,1,1,1,1,1,1,1,1,1,1,1,1,1,1,4),(0.,0.0460148164544132),
(11.6154215191109,12.6130758144294,13.6107301097479,14.6083844050664,15.6060387003849,
16.6036929957034,17.601347291022,18.5990015863405,19.596655881659,20.5943101769775,
21.591964472296,22.5896187676145,23.587273062933,24.5849273582515,25.58258165357,
26.5802359488886,27.5778902442071,28.5755445395256,29.5731988348441,30.5708531301626,
31.5685074254811,32.5661617207996,33.5638160161181,34.5614703114366,35.5591246067551,
36.5567789020737,37.5544331973922,38.5520874927107,39.5497417880292,40.5473960833477,
41.5450503786662,42.5427046739847,43.5403589693032,44.5380132646217,45.5356675599403,
46.5333218552588,47.5309761505773,48.5286304458958,49.5262847412143,50.5239390365328,
51.5215933318513,52.5192476271698,53.5169019224883,54.5145562178069,55.5122105131254,
56.5098648084439,57.5075191037624,58.5051733990809,59.5028276943994,60.5004819897179,
61.4981362850364,62.4957905803549,63.4934448756734,64.491099170992,65.4887534663105,
66.486407761629,67.4840620569475,68.481716352266,69.4793706475845,70.477024942903,
71.4746792382215,72.4723335335401,73.4699878288586,74.4676421241771,75.4652964194956,
76.4629507148141,77.4606050101326,78.4582593054511,79.4559136007696,80.4535678960881,
81.4512221914066,82.4488764867252,83.4465307820437,84.4441850773622,85.4418393726807,
86.4394936679992,87.4371479633177,88.4348022586362,89.4324565539547,90.4301108492732,
91.4277651445918,92.4254194399103,93.4230737352288,94.4207280305473,95.4183823258658,
96.4160366211843,97.4136909165028,98.4113452118213,99.4089995071398,100.406653802458,
101.404308097777,102.401962393095,103.399616688414,104.397270983732,105.394925279051,
106.392579574369,107.390233869688,108.387888165006,109.385542460325,110.383196755643,
111.380851050962,112.37850534628,113.376159641599,114.373813936918,115.371468232236,
116.369122527555,117.366776822873,118.364431118192,119.36208541351,120.359739708829,
121.357394004147,122.355048299466,123.352702594784,124.350356890103,125.348011185421,
126.34566548074,127.343319776058,128.340974071377,129.338628366695,130.336282662014,
131.333936957332,132.331591252651,133.329245547969,134.326899843288,135.324554138606,
136.322208433925,137.319862729243,138.317517024562,139.31517131988,140.312825615199,
141.310479910517,142.308134205836,143.305788501154,144.303442796473,145.301097091791,
146.29875138711,147.296405682428,148.294059977747,149.291714273065,150.289368568384,
151.287022863702,152.284677159021,153.282331454339,154.279985749658,155.277640044976,
156.275294340295,157.272948635613,158.270602930932,159.268257226251,160.265911521569,
161.263565816888,162.261220112206,163.258874407525,164.256528702843,165.254182998162,
166.25183729348,167.249491588799,168.247145884117,169.244800179436,170.242454474754,
171.240108770073,172.237763065391,173.23541736071,174.233071656028,175.230725951347,
176.228380246665,177.226034541984,178.223688837302,179.221343132621,180.218997427939,
181.216651723258,182.214306018576,183.211960313895,184.209614609213,185.207268904532,
186.20492319985,187.202577495169,188.200231790487,189.197886085806,190.195540381124,
191.193194676443,192.190848971761,193.18850326708,194.186157562398,195.183811857717,
196.181466153035,197.179120448354,198.176774743672,199.174429038991,200.172083334309,
201.169737629628,202.167391924946,203.165046220265,204.162700515584,205.160354810902,
206.158009106221,207.155663401539,208.153317696858,209.150971992176,210.148626287495,
211.146280582813,212.143934878132,213.14158917345,214.139243468769,215.136897764087,
216.134552059406,217.132206354724,218.129860650043,219.127514945361,220.12516924068,
221.122823535998,222.120477831317,223.118132126635,224.115786421954,225.113440717272,
226.111095012591,227.108749307909,228.106403603228,229.104057898546),
 .UNSPECIFIED.);
#173=B_SPLINE_SURFACE_WITH_KNOTS('',3,3,((#12265,#12266,#12267,#12268,#12269,
#12270,#12271,#12272,#12273,#12274,#12275,#12276,#12277,#12278,#12279,#12280,
#12281,#12282,#12283,#12284,#12285,#12286,#12287,#12288,#12289,#12290,#12291,
#12292,#12293,#12294,#12295,#12296,#12297,#12298,#12299,#12300,#12301,#12302,
#12303,#12304,#12305),(#12306,#12307,#12308,#12309,#12310,#12311,#12312,
#12313,#12314,#12315,#12316,#12317,#12318,#12319,#12320,#12321,#12322,#12323,
#12324,#12325,#12326,#12327,#12328,#12329,#12330,#12331,#12332,#12333,#12334,
#12335,#12336,#12337,#12338,#12339,#12340,#12341,#12342,#12343,#12344,#12345,
#12346),(#12347,#12348,#12349,#12350,#12351,#12352,#12353,#12354,#12355,
#12356,#12357,#12358,#12359,#12360,#12361,#12362,#12363,#12364,#12365,#12366,
#12367,#12368,#12369,#12370,#12371,#12372,#12373,#12374,#12375,#12376,#12377,
#12378,#12379,#12380,#12381,#12382,#12383,#12384,#12385,#12386,#12387),
(#12388,#12389,#12390,#12391,#12392,#12393,#12394,#12395,#12396,#12397,
#12398,#12399,#12400,#12401,#12402,#12403,#12404,#12405,#12406,#12407,#12408,
#12409,#12410,#12411,#12412,#12413,#12414,#12415,#12416,#12417,#12418,#12419,
#12420,#12421,#12422,#12423,#12424,#12425,#12426,#12427,#12428)),
 .UNSPECIFIED.,.F.,.F.,.F.,(4,4),(4,1,1,1,1,1,1,1,1,1,1,1,1,1,1,1,1,1,1,
1,1,1,1,1,1,1,1,1,1,1,1,1,1,1,1,1,1,1,4),(0.,0.0448889834294934),(11.8615800042567,
12.8594360281068,13.8572920519568,14.8551480758068,15.8530040996568,16.8508601235068,
17.8487161473568,18.8465721712069,19.8444281950569,20.8422842189069,21.8401402427569,
22.8379962666069,23.8358522904569,24.833708314307,25.831564338157,26.829420362007,
27.827276385857,28.825132409707,29.822988433557,30.8208444574071,31.8187004812571,
32.8165565051071,33.8144125289571,34.8122685528071,35.8101245766571,36.8079806005072,
37.8058366243572,38.8036926482072,39.8015486720572,40.7994046959072,41.7972607197572,
42.7951167436073,43.7929727674573,44.7908287913073,45.7886848151573,46.7865408390073,
47.7843968628573,48.7822528867074,49.7801089105574),.UNSPECIFIED.);
#174=B_SPLINE_SURFACE_WITH_KNOTS('',3,3,((#12558,#12559,#12560,#12561,#12562,
#12563,#12564,#12565,#12566,#12567,#12568,#12569,#12570,#12571,#12572,#12573,
#12574,#12575,#12576,#12577,#12578,#12579,#12580,#12581,#12582,#12583,#12584,
#12585,#12586,#12587,#12588,#12589,#12590,#12591,#12592,#12593,#12594,#12595,
#12596,#12597,#12598),(#12599,#12600,#12601,#12602,#12603,#12604,#12605,
#12606,#12607,#12608,#12609,#12610,#12611,#12612,#12613,#12614,#12615,#12616,
#12617,#12618,#12619,#12620,#12621,#12622,#12623,#12624,#12625,#12626,#12627,
#12628,#12629,#12630,#12631,#12632,#12633,#12634,#12635,#12636,#12637,#12638,
#12639),(#12640,#12641,#12642,#12643,#12644,#12645,#12646,#12647,#12648,
#12649,#12650,#12651,#12652,#12653,#12654,#12655,#12656,#12657,#12658,#12659,
#12660,#12661,#12662,#12663,#12664,#12665,#12666,#12667,#12668,#12669,#12670,
#12671,#12672,#12673,#12674,#12675,#12676,#12677,#12678,#12679,#12680),
(#12681,#12682,#12683,#12684,#12685,#12686,#12687,#12688,#12689,#12690,
#12691,#12692,#12693,#12694,#12695,#12696,#12697,#12698,#12699,#12700,#12701,
#12702,#12703,#12704,#12705,#12706,#12707,#12708,#12709,#12710,#12711,#12712,
#12713,#12714,#12715,#12716,#12717,#12718,#12719,#12720,#12721)),
 .UNSPECIFIED.,.F.,.F.,.F.,(4,4),(4,1,1,1,1,1,1,1,1,1,1,1,1,1,1,1,1,1,1,
1,1,1,1,1,1,1,1,1,1,1,1,1,1,1,1,1,1,1,4),(0.,0.0448889834294934),(14.398141012777,
15.395997036627,16.393853060477,17.391709084327,18.389565108177,19.3874211320271,
20.3852771558771,21.3831331797271,22.3809892035771,23.3788452274271,24.3767012512771,
25.3745572751272,26.3724132989772,27.3702693228272,28.3681253466772,29.3659813705272,
30.3638373943772,31.3616934182273,32.3595494420773,33.3574054659273,34.3552614897773,
35.3531175136273,36.3509735374774,37.3488295613274,38.3466855851774,39.3445416090274,
40.3423976328774,41.3402536567274,42.3381096805775,43.3359657044275,44.3338217282775,
45.3316777521275,46.3295337759775,47.3273897998275,48.3252458236776,49.3231018475276,
50.3209578713776,51.3188138952276,52.3166699190776),.UNSPECIFIED.);
#175=B_SPLINE_CURVE_WITH_KNOTS('',3,(#7263,#7264,#7265,#7266,#7267,#7268,
#7269,#7270,#7271,#7272),.UNSPECIFIED.,.F.,.F.,(4,3,3,4),(-4.0925417488383,
-3.99061718127404,-2.99296288595553,-2.06514013327811),.UNSPECIFIED.);
#176=B_SPLINE_CURVE_WITH_KNOTS('',3,(#7275,#7276,#7277,#7278,#7279,#7280,
#7281),.UNSPECIFIED.,.F.,.F.,(4,3,4),(0.,0.997654295318505,1.11419103802989),
 .UNSPECIFIED.);
#177=B_SPLINE_CURVE_WITH_KNOTS('',3,(#7286,#7287,#7288,#7289,#7290,#7291,
#7292,#7293,#7294,#7295,#7296,#7297,#7298,#7299,#7300,#7301,#7302,#7303,
#7304,#7305,#7306,#7307),.UNSPECIFIED.,.F.,.F.,(4,3,3,3,3,3,3,4),(-10.3757270560179,
-9.97654295318511,-8.9788886578666,-7.98123436254809,-6.98358006722958,
-5.98592577191107,-4.98827147659255,-4.0925417488383),.UNSPECIFIED.);
#178=B_SPLINE_CURVE_WITH_KNOTS('',3,(#7308,#7309,#7310,#7311,#7312,#7313,
#7314,#7315,#7316,#7317,#7318,#7319,#7320,#7321,#7322,#7323,#7324,#7325,
#7326,#7327,#7328,#7329),.UNSPECIFIED.,.F.,.F.,(4,3,3,3,3,3,3,4),(1.11419103802989,
1.99530859063702,2.99296288595553,3.99061718127404,4.98827147659255,5.98592577191106,
6.98358006722958,7.39737634520948),.UNSPECIFIED.);
#179=B_SPLINE_CURVE_WITH_KNOTS('',3,(#7334,#7335,#7336,#7337,#7338,#7339,
#7340,#7341,#7342,#7343,#7344,#7345,#7346,#7347,#7348,#7349,#7350,#7351,
#7352,#7353,#7354,#7355),.UNSPECIFIED.,.F.,.F.,(4,3,3,3,3,3,3,4),(-16.6589123631975,
-15.9624687250962,-14.9648144297777,-13.9671601344592,-12.9695058391406,
-11.9718515438221,-10.9741972485036,-10.3757270560179),.UNSPECIFIED.);
#180=B_SPLINE_CURVE_WITH_KNOTS('',3,(#7356,#7357,#7358,#7359,#7360,#7361,
#7362,#7363,#7364,#7365,#7366,#7367,#7368,#7369,#7370,#7371,#7372,#7373,
#7374,#7375,#7376,#7377),.UNSPECIFIED.,.F.,.F.,(4,3,3,3,3,3,3,4),(7.39737634520948,
7.98123436254809,8.97888865786661,9.97654295318512,10.9741972485036,11.9718515438221,
12.9695058391407,13.6805616523891),.UNSPECIFIED.);
#181=B_SPLINE_CURVE_WITH_KNOTS('',3,(#7382,#7383,#7384,#7385,#7386,#7387,
#7388,#7389,#7390,#7391,#7392,#7393,#7394,#7395,#7396,#7397,#7398,#7399,
#7400,#7401,#7402,#7403),.UNSPECIFIED.,.F.,.F.,(4,3,3,3,3,3,3,4),(-22.9420976703771,
-21.9483944970072,-20.9507402016887,-19.9530859063702,-18.9554316110517,
-17.9577773157332,-16.9601230204147,-16.6589123631975),.UNSPECIFIED.);
#182=B_SPLINE_CURVE_WITH_KNOTS('',3,(#7404,#7405,#7406,#7407,#7408,#7409,
#7410,#7411,#7412,#7413,#7414,#7415,#7416,#7417,#7418,#7419,#7420,#7421,
#7422,#7423,#7424,#7425,#7426,#7427,#7428),.UNSPECIFIED.,.F.,.F.,(4,3,3,
3,3,3,3,3,4),(13.6805616523891,13.9671601344592,14.9648144297777,15.9624687250962,
16.9601230204147,17.9577773157332,18.9554316110517,19.9530859063702,19.9637469595687),
 .UNSPECIFIED.);
#183=B_SPLINE_CURVE_WITH_KNOTS('',3,(#7433,#7434,#7435,#7436,#7437,#7438,
#7439,#7440,#7441,#7442,#7443,#7444,#7445,#7446,#7447,#7448,#7449,#7450,
#7451,#7452,#7453,#7454),.UNSPECIFIED.,.F.,.F.,(4,3,3,3,3,3,3,4),(-29.2252829775566,
-28.9319745642368,-27.9343202689183,-26.9366659735998,-25.9390116782813,
-24.9413573829628,-23.9437030876443,-22.9420976703771),.UNSPECIFIED.);
#184=B_SPLINE_CURVE_WITH_KNOTS('',3,(#7455,#7456,#7457,#7458,#7459,#7460,
#7461,#7462,#7463,#7464,#7465,#7466,#7467,#7468,#7469,#7470,#7471,#7472,
#7473,#7474,#7475,#7476),.UNSPECIFIED.,.F.,.F.,(4,3,3,3,3,3,3,4),(19.9637469595687,
20.9507402016887,21.9483944970072,22.9460487923258,23.9437030876443,24.9413573829628,
25.9390116782813,26.2469322667482),.UNSPECIFIED.);
#185=B_SPLINE_CURVE_WITH_KNOTS('',3,(#7481,#7482,#7483,#7484,#7485,#7486,
#7487,#7488,#7489,#7490,#7491,#7492,#7493,#7494,#7495,#7496,#7497,#7498,
#7499,#7500,#7501,#7502),.UNSPECIFIED.,.F.,.F.,(4,3,3,3,3,3,3,4),(-35.5084682847362,
-34.9179003361479,-33.9202460408294,-32.9225917455109,-31.9249374501923,
-30.9272831548738,-29.9296288595553,-29.2252829775566),.UNSPECIFIED.);
#186=B_SPLINE_CURVE_WITH_KNOTS('',3,(#7503,#7504,#7505,#7506,#7507,#7508,
#7509,#7510,#7511,#7512,#7513,#7514,#7515,#7516,#7517,#7518,#7519,#7520,
#7521,#7522,#7523,#7524),.UNSPECIFIED.,.F.,.F.,(4,3,3,3,3,3,3,4),(26.2469322667482,
26.9366659735998,27.9343202689183,28.9319745642368,29.9296288595553,30.9272831548739,
31.9249374501924,32.5301175739278),.UNSPECIFIED.);
#187=B_SPLINE_CURVE_WITH_KNOTS('',3,(#7529,#7530,#7531,#7532,#7533,#7534,
#7535,#7536,#7537,#7538,#7539,#7540,#7541,#7542,#7543,#7544,#7545,#7546,
#7547,#7548,#7549,#7550),.UNSPECIFIED.,.F.,.F.,(4,3,3,3,3,3,3,4),(-41.7916535919158,
-40.903826108059,-39.9061718127404,-38.9085175174219,-37.9108632221034,
-36.9132089267849,-35.9155546314664,-35.5084682847362),.UNSPECIFIED.);
#188=B_SPLINE_CURVE_WITH_KNOTS('',3,(#7551,#7552,#7553,#7554,#7555,#7556,
#7557,#7558,#7559,#7560,#7561,#7562,#7563,#7564,#7565,#7566,#7567,#7568,
#7569,#7570,#7571,#7572),.UNSPECIFIED.,.F.,.F.,(4,3,3,3,3,3,3,4),(32.5301175739278,
32.9225917455109,33.9202460408294,34.9179003361479,35.9155546314664,36.9132089267849,
37.9108632221034,38.8133028811074),.UNSPECIFIED.);
#189=B_SPLINE_CURVE_WITH_KNOTS('',3,(#7577,#7578,#7579,#7580,#7581,#7582,
#7583,#7584,#7585,#7586,#7587,#7588,#7589,#7590,#7591,#7592,#7593,#7594,
#7595,#7596,#7597,#7598,#7599,#7600,#7601),.UNSPECIFIED.,.F.,.F.,(4,3,3,
3,3,3,3,3,4),(-48.0748388990954,-47.8874061752885,-46.88975187997,-45.8920975846515,
-44.894443289333,-43.8967889940145,-42.899134698696,-41.9014804033775,-41.7916535919158),
 .UNSPECIFIED.);
#190=B_SPLINE_CURVE_WITH_KNOTS('',3,(#7602,#7603,#7604,#7605,#7606,#7607,
#7608,#7609,#7610,#7611,#7612,#7613,#7614,#7615,#7616,#7617,#7618,#7619,
#7620,#7621,#7622,#7623,#7624,#7625,#7626),.UNSPECIFIED.,.F.,.F.,(4,3,3,
3,3,3,3,3,4),(38.8133028811074,38.908517517422,39.9061718127405,40.903826108059,
41.9014804033775,42.899134698696,43.8967889940145,44.894443289333,45.096488188287),
 .UNSPECIFIED.);
#191=B_SPLINE_CURVE_WITH_KNOTS('',3,(#7631,#7632,#7633,#7634,#7635,#7636,
#7637,#7638,#7639,#7640,#7641,#7642,#7643,#7644,#7645,#7646,#7647,#7648,
#7649,#7650,#7651,#7652),.UNSPECIFIED.,.F.,.F.,(4,3,3,3,3,3,3,4),(-54.358024206275,
-53.8733319471996,-52.8756776518811,-51.8780233565626,-50.8803690612441,
-49.8827147659256,-48.885060470607,-48.0748388990954),.UNSPECIFIED.);
#192=B_SPLINE_CURVE_WITH_KNOTS('',3,(#7653,#7654,#7655,#7656,#7657,#7658,
#7659,#7660,#7661,#7662,#7663,#7664,#7665,#7666,#7667,#7668,#7669,#7670,
#7671,#7672,#7673,#7674),.UNSPECIFIED.,.F.,.F.,(4,3,3,3,3,3,3,4),(45.096488188287,
45.8920975846515,46.8897518799701,47.8874061752886,48.8850604706071,49.8827147659256,
50.8803690612441,51.3796734954666),.UNSPECIFIED.);
#193=B_SPLINE_CURVE_WITH_KNOTS('',3,(#7679,#7680,#7681,#7682,#7683,#7684,
#7685,#7686,#7687,#7688,#7689,#7690,#7691,#7692,#7693,#7694,#7695,#7696,
#7697,#7698,#7699,#7700),.UNSPECIFIED.,.F.,.F.,(4,3,3,3,3,3,3,4),(-60.6412095134546,
-59.8592577191107,-58.8616034237921,-57.8639491284736,-56.8662948331551,
-55.8686405378366,-54.8709862425181,-54.358024206275),.UNSPECIFIED.);
#194=B_SPLINE_CURVE_WITH_KNOTS('',3,(#7701,#7702,#7703,#7704,#7705,#7706,
#7707,#7708,#7709,#7710,#7711,#7712,#7713,#7714,#7715,#7716,#7717,#7718,
#7719,#7720,#7721,#7722),.UNSPECIFIED.,.F.,.F.,(4,3,3,3,3,3,3,4),(51.3796734954666,
51.8780233565626,52.8756776518811,53.8733319471996,54.8709862425181,55.8686405378366,
56.8662948331552,57.6628588026462),.UNSPECIFIED.);
#195=B_SPLINE_CURVE_WITH_KNOTS('',3,(#7727,#7728,#7729,#7730,#7731,#7732,
#7733,#7734,#7735,#7736,#7737,#7738,#7739,#7740,#7741,#7742,#7743,#7744,
#7745,#7746,#7747,#7748,#7749,#7750,#7751),.UNSPECIFIED.,.F.,.F.,(4,3,3,
3,3,3,3,3,4),(-66.9243948206342,-66.8428377863402,-65.8451834910217,-64.8475291957032,
-63.8498749003847,-62.8522206050662,-61.8545663097477,-60.8569120144292,
-60.6412095134546),.UNSPECIFIED.);
#196=B_SPLINE_CURVE_WITH_KNOTS('',3,(#7752,#7753,#7754,#7755,#7756,#7757,
#7758,#7759,#7760,#7761,#7762,#7763,#7764,#7765,#7766,#7767,#7768,#7769,
#7770,#7771,#7772,#7773,#7774,#7775,#7776),.UNSPECIFIED.,.F.,.F.,(4,3,3,
3,3,3,3,3,4),(57.6628588026462,57.8639491284737,58.8616034237922,59.8592577191107,
60.8569120144292,61.8545663097477,62.8522206050662,63.8498749003847,63.9460441098258),
 .UNSPECIFIED.);
#197=B_SPLINE_CURVE_WITH_KNOTS('',3,(#7781,#7782,#7783,#7784,#7785,#7786,
#7787,#7788,#7789,#7790,#7791,#7792,#7793,#7794,#7795,#7796,#7797,#7798,
#7799,#7800,#7801,#7802),.UNSPECIFIED.,.F.,.F.,(4,3,3,3,3,3,3,4),(-73.2075801278138,
-72.8287635582513,-71.8311092629328,-70.8334549676143,-69.8358006722958,
-68.8381463769772,-67.8404920816587,-66.9243948206342),.UNSPECIFIED.);
#198=B_SPLINE_CURVE_WITH_KNOTS('',3,(#7803,#7804,#7805,#7806,#7807,#7808,
#7809,#7810,#7811,#7812,#7813,#7814,#7815,#7816,#7817,#7818,#7819,#7820,
#7821,#7822,#7823,#7824),.UNSPECIFIED.,.F.,.F.,(4,3,3,3,3,3,3,4),(63.9460441098258,
64.8475291957032,65.8451834910218,66.8428377863403,67.8404920816588,68.8381463769773,
69.8358006722958,70.2292294170054),.UNSPECIFIED.);
#199=B_SPLINE_CURVE_WITH_KNOTS('',3,(#7829,#7830,#7831,#7832,#7833,#7834,
#7835,#7836,#7837,#7838,#7839,#7840,#7841,#7842,#7843,#7844,#7845,#7846,
#7847,#7848,#7849,#7850),.UNSPECIFIED.,.F.,.F.,(4,3,3,3,3,3,3,4),(-79.4907654349934,
-78.8146893301624,-77.8170350348439,-76.8193807395253,-75.8217264442068,
-74.8240721488883,-73.8264178535698,-73.2075801278138),.UNSPECIFIED.);
#200=B_SPLINE_CURVE_WITH_KNOTS('',3,(#7851,#7852,#7853,#7854,#7855,#7856,
#7857,#7858,#7859,#7860,#7861,#7862,#7863,#7864,#7865,#7866,#7867,#7868,
#7869,#7870,#7871,#7872),.UNSPECIFIED.,.F.,.F.,(4,3,3,3,3,3,3,4),(70.2292294170054,
70.8334549676143,71.8311092629328,72.8287635582514,73.8264178535699,74.8240721488884,
75.8217264442069,76.512414724185),.UNSPECIFIED.);
#201=B_SPLINE_CURVE_WITH_KNOTS('',3,(#7877,#7878,#7879,#7880,#7881,#7882,
#7883,#7884,#7885,#7886,#7887,#7888,#7889,#7890,#7891,#7892,#7893,#7894,
#7895,#7896,#7897,#7898),.UNSPECIFIED.,.F.,.F.,(4,3,3,3,3,3,3,4),(-85.773950742173,
-84.8006151020734,-83.8029608067549,-82.8053065114364,-81.8076522161179,
-80.8099979207994,-79.8123436254809,-79.4907654349934),.UNSPECIFIED.);
#202=B_SPLINE_CURVE_WITH_KNOTS('',3,(#7899,#7900,#7901,#7902,#7903,#7904,
#7905,#7906,#7907,#7908,#7909,#7910,#7911,#7912,#7913,#7914,#7915,#7916,
#7917,#7918,#7919,#7920),.UNSPECIFIED.,.F.,.F.,(4,3,3,3,3,3,3,4),(76.512414724185,
76.8193807395254,77.8170350348439,78.8146893301624,79.8123436254809,80.8099979207994,
81.8076522161179,82.7956000313646),.UNSPECIFIED.);
#203=B_SPLINE_CURVE_WITH_KNOTS('',3,(#7925,#7926,#7927,#7928,#7929,#7930,
#7931,#7932,#7933,#7934,#7935,#7936,#7937,#7938,#7939,#7940,#7941,#7942,
#7943,#7944,#7945,#7946,#7947,#7948,#7949),.UNSPECIFIED.,.F.,.F.,(4,3,3,
3,3,3,3,3,4),(-92.0571360493526,-91.784195169303,-90.7865408739845,-89.788886578666,
-88.7912322833475,-87.793577988029,-86.7959236927104,-85.7982693973919,
-85.773950742173),.UNSPECIFIED.);
#204=B_SPLINE_CURVE_WITH_KNOTS('',3,(#7950,#7951,#7952,#7953,#7954,#7955,
#7956,#7957,#7958,#7959,#7960,#7961,#7962,#7963,#7964,#7965,#7966,#7967,
#7968,#7969,#7970,#7971,#7972,#7973,#7974),.UNSPECIFIED.,.F.,.F.,(4,3,3,
3,3,3,3,3,4),(82.7956000313646,82.8053065114364,83.802960806755,84.8006151020735,
85.798269397392,86.7959236927105,87.793577988029,88.7912322833475,89.0787853385442),
 .UNSPECIFIED.);
#205=B_SPLINE_CURVE_WITH_KNOTS('',3,(#7979,#7980,#7981,#7982,#7983,#7984,
#7985,#7986,#7987,#7988,#7989,#7990,#7991,#7992,#7993,#7994,#7995,#7996,
#7997,#7998,#7999,#8000),.UNSPECIFIED.,.F.,.F.,(4,3,3,3,3,3,3,4),(-98.3403213565322,
-97.7701209412141,-96.7724666458956,-95.7748123505771,-94.7771580552585,
-93.77950375994,-92.7818494646215,-92.0571360493526),.UNSPECIFIED.);
#206=B_SPLINE_CURVE_WITH_KNOTS('',3,(#8001,#8002,#8003,#8004,#8005,#8006,
#8007,#8008,#8009,#8010,#8011,#8012,#8013,#8014,#8015,#8016,#8017,#8018,
#8019,#8020,#8021,#8022),.UNSPECIFIED.,.F.,.F.,(4,3,3,3,3,3,3,4),(89.0787853385442,
89.7888865786661,90.7865408739846,91.7841951693031,92.7818494646216,93.7795037599401,
94.7771580552586,95.3619706457238),.UNSPECIFIED.);
#207=B_SPLINE_CURVE_WITH_KNOTS('',3,(#8027,#8028,#8029,#8030,#8031,#8032,
#8033,#8034,#8035,#8036,#8037,#8038,#8039,#8040,#8041,#8042,#8043,#8044,
#8045,#8046,#8047,#8048),.UNSPECIFIED.,.F.,.F.,(4,3,3,3,3,3,3,4),(-104.623506663712,
-103.756046713125,-102.758392417807,-101.760738122488,-100.76308382717,
-99.7654295318511,-98.7677752365326,-98.3403213565322),.UNSPECIFIED.);
#208=B_SPLINE_CURVE_WITH_KNOTS('',3,(#8049,#8050,#8051,#8052,#8053,#8054,
#8055,#8056,#8057,#8058,#8059,#8060,#8061,#8062,#8063,#8064,#8065,#8066,
#8067,#8068,#8069,#8070),.UNSPECIFIED.,.F.,.F.,(4,3,3,3,3,3,3,4),(95.3619706457238,
95.7748123505771,96.7724666458956,97.7701209412141,98.7677752365326,99.7654295318512,
100.76308382717,101.645155952903),.UNSPECIFIED.);
#209=B_SPLINE_CURVE_WITH_KNOTS('',3,(#8075,#8076,#8077,#8078,#8079,#8080,
#8081,#8082,#8083,#8084,#8085,#8086,#8087,#8088,#8089,#8090,#8091,#8092,
#8093,#8094,#8095,#8096,#8097,#8098,#8099),.UNSPECIFIED.,.F.,.F.,(4,3,3,
3,3,3,3,3,4),(-110.906691970891,-110.739626780355,-109.741972485036,-108.744318189718,
-107.746663894399,-106.749009599081,-105.751355303762,-104.753701008444,
-104.623506663712),.UNSPECIFIED.);
#210=B_SPLINE_CURVE_WITH_KNOTS('',3,(#8100,#8101,#8102,#8103,#8104,#8105,
#8106,#8107,#8108,#8109,#8110,#8111,#8112,#8113,#8114,#8115,#8116,#8117,
#8118,#8119,#8120,#8121,#8122,#8123,#8124),.UNSPECIFIED.,.F.,.F.,(4,3,3,
3,3,3,3,3,4),(101.645155952903,101.760738122488,102.758392417807,103.756046713125,
104.753701008444,105.751355303762,106.749009599081,107.746663894399,107.928341260083),
 .UNSPECIFIED.);
#211=B_SPLINE_CURVE_WITH_KNOTS('',3,(#8129,#8130,#8131,#8132,#8133,#8134,
#8135,#8136,#8137,#8138,#8139,#8140,#8141,#8142,#8143,#8144,#8145,#8146,
#8147,#8148,#8149,#8150),.UNSPECIFIED.,.F.,.F.,(4,3,3,3,3,3,3,4),(-117.189877278071,
-116.725552552266,-115.727898256947,-114.730243961629,-113.73258966631,
-112.734935370992,-111.737281075673,-110.906691970891),.UNSPECIFIED.);
#212=B_SPLINE_CURVE_WITH_KNOTS('',3,(#8151,#8152,#8153,#8154,#8155,#8156,
#8157,#8158,#8159,#8160,#8161,#8162,#8163,#8164,#8165,#8166,#8167,#8168,
#8169,#8170,#8171,#8172),.UNSPECIFIED.,.F.,.F.,(4,3,3,3,3,3,3,4),(107.928341260083,
108.744318189718,109.741972485036,110.739626780355,111.737281075673,112.734935370992,
113.73258966631,114.211526567263),.UNSPECIFIED.);
#213=B_SPLINE_CURVE_WITH_KNOTS('',3,(#8177,#8178,#8179,#8180,#8181,#8182,
#8183,#8184,#8185,#8186,#8187,#8188,#8189,#8190,#8191,#8192,#8193,#8194,
#8195,#8196,#8197,#8198),.UNSPECIFIED.,.F.,.F.,(4,3,3,3,3,3,3,4),(-123.473062585251,
-122.711478324177,-121.713824028858,-120.71616973354,-119.718515438221,
-118.720861142903,-117.723206847584,-117.189877278071),.UNSPECIFIED.);
#214=B_SPLINE_CURVE_WITH_KNOTS('',3,(#8199,#8200,#8201,#8202,#8203,#8204,
#8205,#8206,#8207,#8208,#8209,#8210,#8211,#8212,#8213,#8214,#8215,#8216,
#8217,#8218,#8219,#8220),.UNSPECIFIED.,.F.,.F.,(4,3,3,3,3,3,3,4),(114.211526567263,
114.730243961629,115.727898256947,116.725552552266,117.723206847584,118.720861142903,
119.718515438221,120.494711874442),.UNSPECIFIED.);
#215=B_SPLINE_CURVE_WITH_KNOTS('',3,(#8225,#8226,#8227,#8228,#8229,#8230,
#8231,#8232,#8233,#8234,#8235,#8236,#8237,#8238,#8239,#8240,#8241,#8242,
#8243,#8244,#8245,#8246,#8247,#8248,#8249),.UNSPECIFIED.,.F.,.F.,(4,3,3,
3,3,3,3,3,4),(-129.75624789243,-129.695058391406,-128.697404096088,-127.699749800769,
-126.702095505451,-125.704441210132,-124.706786914814,-123.709132619495,
-123.473062585251),.UNSPECIFIED.);
#216=B_SPLINE_CURVE_WITH_KNOTS('',3,(#8250,#8251,#8252,#8253,#8254,#8255,
#8256,#8257,#8258,#8259,#8260,#8261,#8262,#8263,#8264,#8265,#8266,#8267,
#8268,#8269,#8270,#8271,#8272,#8273,#8274),.UNSPECIFIED.,.F.,.F.,(4,3,3,
3,3,3,3,3,4),(120.494711874442,120.71616973354,121.713824028858,122.711478324177,
123.709132619495,124.706786914814,125.704441210132,126.702095505451,126.777897181622),
 .UNSPECIFIED.);
#217=B_SPLINE_CURVE_WITH_KNOTS('',3,(#8279,#8280,#8281,#8282,#8283,#8284,
#8285,#8286,#8287,#8288,#8289,#8290,#8291,#8292,#8293,#8294,#8295,#8296,
#8297,#8298,#8299,#8300),.UNSPECIFIED.,.F.,.F.,(4,3,3,3,3,3,3,4),(-136.03943319961,
-135.680984163318,-134.683329867999,-133.68567557268,-132.688021277362,
-131.690366982043,-130.692712686725,-129.75624789243),.UNSPECIFIED.);
#218=B_SPLINE_CURVE_WITH_KNOTS('',3,(#8301,#8302,#8303,#8304,#8305,#8306,
#8307,#8308,#8309,#8310,#8311,#8312,#8313,#8314,#8315,#8316,#8317,#8318,
#8319,#8320,#8321,#8322),.UNSPECIFIED.,.F.,.F.,(4,3,3,3,3,3,3,4),(126.777897181622,
127.699749800769,128.697404096088,129.695058391406,130.692712686725,131.690366982044,
132.688021277362,133.061082488801),.UNSPECIFIED.);
#219=B_SPLINE_CURVE_WITH_KNOTS('',3,(#8327,#8328,#8329,#8330,#8331,#8332,
#8333,#8334,#8335,#8336,#8337,#8338,#8339,#8340,#8341,#8342,#8343,#8344,
#8345,#8346,#8347,#8348),.UNSPECIFIED.,.F.,.F.,(4,3,3,3,3,3,3,4),(-142.322618506789,
-141.666909935229,-140.66925563991,-139.671601344592,-138.673947049273,
-137.676292753955,-136.678638458636,-136.03943319961),.UNSPECIFIED.);
#220=B_SPLINE_CURVE_WITH_KNOTS('',3,(#8349,#8350,#8351,#8352,#8353,#8354,
#8355,#8356,#8357,#8358,#8359,#8360,#8361,#8362,#8363,#8364,#8365,#8366,
#8367,#8368,#8369,#8370),.UNSPECIFIED.,.F.,.F.,(4,3,3,3,3,3,3,4),(133.061082488801,
133.685675572681,134.683329867999,135.680984163318,136.678638458636,137.676292753955,
138.673947049273,139.344267795981),.UNSPECIFIED.);
#221=B_SPLINE_CURVE_WITH_KNOTS('',3,(#8375,#8376,#8377,#8378,#8379,#8380,
#8381,#8382,#8383,#8384,#8385,#8386,#8387,#8388,#8389,#8390,#8391,#8392,
#8393,#8394,#8395,#8396),.UNSPECIFIED.,.F.,.F.,(4,3,3,3,3,3,3,4),(-148.605803813969,
-147.65283570714,-146.655181411821,-145.657527116503,-144.659872821184,
-143.662218525866,-142.664564230547,-142.322618506789),.UNSPECIFIED.);
#222=B_SPLINE_CURVE_WITH_KNOTS('',3,(#8397,#8398,#8399,#8400,#8401,#8402,
#8403,#8404,#8405,#8406,#8407,#8408,#8409,#8410,#8411,#8412,#8413,#8414,
#8415,#8416,#8417,#8418),.UNSPECIFIED.,.F.,.F.,(4,3,3,3,3,3,3,4),(139.344267795981,
139.671601344592,140.66925563991,141.666909935229,142.664564230547,143.662218525866,
144.659872821184,145.62745310316),.UNSPECIFIED.);
#223=B_SPLINE_CURVE_WITH_KNOTS('',3,(#8423,#8424,#8425,#8426,#8427,#8428,
#8429,#8430,#8431,#8432,#8433,#8434,#8435,#8436,#8437,#8438,#8439,#8440,
#8441,#8442,#8443,#8444,#8445,#8446,#8447),.UNSPECIFIED.,.F.,.F.,(4,3,3,
3,3,3,3,3,4),(-154.888989121148,-154.636415774369,-153.638761479051,-152.641107183732,
-151.643452888414,-150.645798593095,-149.648144297777,-148.650490002458,
-148.605803813969),.UNSPECIFIED.);
#224=B_SPLINE_CURVE_WITH_KNOTS('',3,(#8448,#8449,#8450,#8451,#8452,#8453,
#8454,#8455,#8456,#8457,#8458,#8459,#8460,#8461,#8462,#8463,#8464,#8465,
#8466,#8467,#8468,#8469,#8470,#8471,#8472),.UNSPECIFIED.,.F.,.F.,(4,3,3,
3,3,3,3,3,4),(145.62745310316,145.657527116503,146.655181411821,147.65283570714,
148.650490002458,149.648144297777,150.645798593095,151.643452888414,151.91063841034),
 .UNSPECIFIED.);
#225=B_SPLINE_CURVE_WITH_KNOTS('',3,(#8477,#8478,#8479,#8480,#8481,#8482,
#8483,#8484,#8485,#8486,#8487,#8488,#8489,#8490,#8491,#8492,#8493,#8494,
#8495,#8496,#8497,#8498),.UNSPECIFIED.,.F.,.F.,(4,3,3,3,3,3,3,4),(-161.172174428328,
-160.62234154628,-159.624687250962,-158.627032955643,-157.629378660325,
-156.631724365006,-155.634070069688,-154.888989121148),.UNSPECIFIED.);
#226=B_SPLINE_CURVE_WITH_KNOTS('',3,(#8499,#8500,#8501,#8502,#8503,#8504,
#8505,#8506,#8507,#8508,#8509,#8510,#8511,#8512,#8513,#8514,#8515,#8516,
#8517,#8518,#8519,#8520),.UNSPECIFIED.,.F.,.F.,(4,3,3,3,3,3,3,4),(151.91063841034,
152.641107183732,153.638761479051,154.636415774369,155.634070069688,156.631724365006,
157.629378660325,158.19382371752),.UNSPECIFIED.);
#227=B_SPLINE_CURVE_WITH_KNOTS('',3,(#8525,#8526,#8527,#8528,#8529,#8530,
#8531,#8532,#8533,#8534,#8535,#8536,#8537,#8538,#8539,#8540,#8541,#8542,
#8543,#8544,#8545,#8546),.UNSPECIFIED.,.F.,.F.,(4,3,3,3,3,3,3,4),(-167.455359735508,
-166.608267318191,-165.610613022873,-164.612958727554,-163.615304432236,
-162.617650136917,-161.619995841599,-161.172174428328),.UNSPECIFIED.);
#228=B_SPLINE_CURVE_WITH_KNOTS('',3,(#8547,#8548,#8549,#8550,#8551,#8552,
#8553,#8554,#8555,#8556,#8557,#8558,#8559,#8560,#8561,#8562,#8563,#8564,
#8565,#8566,#8567,#8568),.UNSPECIFIED.,.F.,.F.,(4,3,3,3,3,3,3,4),(158.19382371752,
158.627032955643,159.624687250962,160.62234154628,161.619995841599,162.617650136917,
163.615304432236,164.477009024699),.UNSPECIFIED.);
#229=B_SPLINE_CURVE_WITH_KNOTS('',3,(#8573,#8574,#8575,#8576,#8577,#8578,
#8579,#8580,#8581,#8582,#8583,#8584,#8585,#8586,#8587,#8588,#8589,#8590,
#8591,#8592,#8593,#8594,#8595,#8596,#8597),.UNSPECIFIED.,.F.,.F.,(4,3,3,
3,3,3,3,3,4),(-173.738545042687,-173.591847385421,-172.594193090102,-171.596538794784,
-170.598884499465,-169.601230204147,-168.603575908828,-167.60592161351,
-167.455359735508),.UNSPECIFIED.);
#230=B_SPLINE_CURVE_WITH_KNOTS('',3,(#8598,#8599,#8600,#8601,#8602,#8603,
#8604,#8605,#8606,#8607,#8608,#8609,#8610,#8611,#8612,#8613,#8614,#8615,
#8616,#8617,#8618,#8619,#8620,#8621,#8622),.UNSPECIFIED.,.F.,.F.,(4,3,3,
3,3,3,3,3,4),(164.477009024699,164.612958727554,165.610613022873,166.608267318191,
167.60592161351,168.603575908828,169.601230204147,170.598884499465,170.760194331879),
 .UNSPECIFIED.);
#231=B_SPLINE_CURVE_WITH_KNOTS('',3,(#8627,#8628,#8629,#8630,#8631,#8632,
#8633,#8634,#8635,#8636,#8637,#8638,#8639,#8640,#8641,#8642,#8643,#8644,
#8645,#8646,#8647,#8648),.UNSPECIFIED.,.F.,.F.,(4,3,3,3,3,3,3,4),(-180.021730349867,
-179.577773157332,-178.580118862013,-177.582464566695,-176.584810271376,
-175.587155976058,-174.589501680739,-173.738545042687),.UNSPECIFIED.);
#232=B_SPLINE_CURVE_WITH_KNOTS('',3,(#8649,#8650,#8651,#8652,#8653,#8654,
#8655,#8656,#8657,#8658,#8659,#8660,#8661,#8662,#8663,#8664,#8665,#8666,
#8667,#8668,#8669,#8670),.UNSPECIFIED.,.F.,.F.,(4,3,3,3,3,3,3,4),(170.760194331879,
171.596538794784,172.594193090102,173.591847385421,174.58950168074,175.587155976058,
176.584810271377,177.043379639058),.UNSPECIFIED.);
#233=B_SPLINE_CURVE_WITH_KNOTS('',3,(#8675,#8676,#8677,#8678,#8679,#8680,
#8681,#8682,#8683,#8684,#8685,#8686,#8687,#8688,#8689,#8690,#8691,#8692,
#8693,#8694,#8695,#8696),.UNSPECIFIED.,.F.,.F.,(4,3,3,3,3,3,3,4),(-186.304915657046,
-185.563698929243,-184.566044633925,-183.568390338606,-182.570736043288,
-181.573081747969,-180.575427452651,-180.021730349867),.UNSPECIFIED.);
#234=B_SPLINE_CURVE_WITH_KNOTS('',3,(#8697,#8698,#8699,#8700,#8701,#8702,
#8703,#8704,#8705,#8706,#8707,#8708,#8709,#8710,#8711,#8712,#8713,#8714,
#8715,#8716,#8717,#8718),.UNSPECIFIED.,.F.,.F.,(4,3,3,3,3,3,3,4),(177.043379639058,
177.582464566695,178.580118862014,179.577773157332,180.575427452651,181.573081747969,
182.570736043288,183.326564946238),.UNSPECIFIED.);
#235=B_SPLINE_CURVE_WITH_KNOTS('',3,(#8723,#8724,#8725,#8726,#8727,#8728,
#8729,#8730,#8731,#8732,#8733,#8734,#8735,#8736,#8737,#8738,#8739,#8740,
#8741,#8742,#8743,#8744,#8745,#8746,#8747),.UNSPECIFIED.,.F.,.F.,(4,3,3,
3,3,3,3,3,4),(-192.588100964226,-192.547278996473,-191.549624701154,-190.551970405836,
-189.554316110517,-188.556661815199,-187.55900751988,-186.561353224562,
-186.304915657046),.UNSPECIFIED.);
#236=B_SPLINE_CURVE_WITH_KNOTS('',3,(#8748,#8749,#8750,#8751,#8752,#8753,
#8754,#8755,#8756,#8757,#8758,#8759,#8760,#8761,#8762,#8763,#8764,#8765,
#8766,#8767,#8768,#8769,#8770,#8771,#8772),.UNSPECIFIED.,.F.,.F.,(4,3,3,
3,3,3,3,3,4),(183.326564946238,183.568390338606,184.566044633925,185.563698929243,
186.561353224562,187.55900751988,188.556661815199,189.554316110517,189.609750253417),
 .UNSPECIFIED.);
#237=B_SPLINE_CURVE_WITH_KNOTS('',3,(#8777,#8778,#8779,#8780,#8781,#8782,
#8783,#8784,#8785,#8786,#8787,#8788,#8789,#8790,#8791,#8792,#8793,#8794,
#8795,#8796,#8797,#8798),.UNSPECIFIED.,.F.,.F.,(4,3,3,3,3,3,3,4),(-198.871286271405,
-198.533204768384,-197.535550473065,-196.537896177747,-195.540241882428,
-194.54258758711,-193.544933291791,-192.588100964226),.UNSPECIFIED.);
#238=B_SPLINE_CURVE_WITH_KNOTS('',3,(#8799,#8800,#8801,#8802,#8803,#8804,
#8805,#8806,#8807,#8808,#8809,#8810,#8811,#8812,#8813,#8814,#8815,#8816,
#8817,#8818,#8819,#8820),.UNSPECIFIED.,.F.,.F.,(4,3,3,3,3,3,3,4),(189.609750253417,
190.551970405836,191.549624701154,192.547278996473,193.544933291791,194.54258758711,
195.540241882428,195.892935560597),.UNSPECIFIED.);
#239=B_SPLINE_CURVE_WITH_KNOTS('',3,(#8825,#8826,#8827,#8828,#8829,#8830,
#8831,#8832,#8833,#8834,#8835,#8836,#8837,#8838,#8839,#8840,#8841,#8842,
#8843,#8844,#8845,#8846),.UNSPECIFIED.,.F.,.F.,(4,3,3,3,3,3,3,4),(-205.154471578585,
-204.519130540295,-203.521476244976,-202.523821949658,-201.526167654339,
-200.528513359021,-199.530859063702,-198.871286271405),.UNSPECIFIED.);
#240=B_SPLINE_CURVE_WITH_KNOTS('',3,(#8847,#8848,#8849,#8850,#8851,#8852,
#8853,#8854,#8855,#8856,#8857,#8858,#8859,#8860,#8861,#8862,#8863,#8864,
#8865,#8866,#8867,#8868),.UNSPECIFIED.,.F.,.F.,(4,3,3,3,3,3,3,4),(195.892935560597,
196.537896177747,197.535550473065,198.533204768384,199.530859063702,200.528513359021,
201.526167654339,202.176120867777),.UNSPECIFIED.);
#241=B_SPLINE_CURVE_WITH_KNOTS('',3,(#8873,#8874,#8875,#8876,#8877,#8878,
#8879,#8880,#8881,#8882,#8883,#8884,#8885,#8886,#8887,#8888,#8889,#8890,
#8891,#8892,#8893,#8894),.UNSPECIFIED.,.F.,.F.,(4,3,3,3,3,3,3,4),(-211.437656885764,
-210.505056312206,-209.507402016887,-208.509747721569,-207.51209342625,
-206.514439130932,-205.516784835613,-205.154471578585),.UNSPECIFIED.);
#242=B_SPLINE_CURVE_WITH_KNOTS('',3,(#8895,#8896,#8897,#8898,#8899,#8900,
#8901,#8902,#8903,#8904,#8905,#8906,#8907,#8908,#8909,#8910,#8911,#8912,
#8913,#8914,#8915,#8916),.UNSPECIFIED.,.F.,.F.,(4,3,3,3,3,3,3,4),(202.176120867777,
202.523821949658,203.521476244976,204.519130540295,205.516784835613,206.514439130932,
207.51209342625,208.459306174956),.UNSPECIFIED.);
#243=B_SPLINE_CURVE_WITH_KNOTS('',3,(#8923,#8924,#8925,#8926,#8927,#8928,
#8929,#8930,#8931,#8932,#8933,#8934,#8935,#8936,#8937,#8938,#8939,#8940,
#8941,#8942,#8943,#8944),.UNSPECIFIED.,.F.,.F.,(4,3,3,3,3,3,3,4),(-217.488636379435,
-216.490982084117,-215.493327788798,-214.49567349348,-213.498019198161,
-212.500364902843,-211.502710607524,-211.437656885764),.UNSPECIFIED.);
#244=B_SPLINE_CURVE_WITH_KNOTS('',3,(#8945,#8946,#8947,#8948,#8949,#8950,
#8951,#8952,#8953,#8954,#8955,#8956,#8957,#8958,#8959,#8960,#8961,#8962,
#8963,#8964,#8965,#8966,#8967,#8968,#8969),.UNSPECIFIED.,.F.,.F.,(4,3,3,
3,3,3,3,3,4),(208.459306174956,208.509747721569,209.507402016887,210.505056312206,
211.502710607524,212.500364902843,213.498019198161,214.49567349348,214.742491482136),
 .UNSPECIFIED.);
#245=B_SPLINE_CURVE_WITH_KNOTS('',3,(#8975,#8976,#8977,#8978,#8979,#8980,
#8981,#8982),.UNSPECIFIED.,.F.,.F.,(4,1,1,1,1,4),(223.053078404875,223.118132126635,
224.115786421954,225.113440717272,226.111095012591,227.038917765268),
 .UNSPECIFIED.);
#246=B_SPLINE_CURVE_WITH_KNOTS('',3,(#8985,#8986,#8987,#8988,#8989,#8990),
 .UNSPECIFIED.,.F.,.F.,(4,1,1,4),(223.053078404875,223.803914711538,224.801569006857,
225.799223302175),.UNSPECIFIED.);
#247=B_SPLINE_CURVE_WITH_KNOTS('',3,(#8995,#8996,#8997,#8998,#8999,#9000,
#9001,#9002,#9003,#9004),.UNSPECIFIED.,.F.,.F.,(4,1,1,1,1,1,1,4),(216.769893097696,
217.132206354724,218.129860650043,219.127514945361,220.12516924068,221.122823535998,
222.120477831317,223.053078404875),.UNSPECIFIED.);
#248=B_SPLINE_CURVE_WITH_KNOTS('',3,(#9005,#9006,#9007,#9008,#9009,#9010,
#9011,#9012,#9013,#9014,#9015),.UNSPECIFIED.,.F.,.F.,(4,1,1,1,1,1,1,1,4),
(216.769893097696,216.820334644309,217.817988939627,218.815643234946,219.813297530264,
220.810951825583,221.808606120901,222.80626041622,223.053078404875),
 .UNSPECIFIED.);
#249=B_SPLINE_CURVE_WITH_KNOTS('',3,(#9020,#9021,#9022,#9023,#9024,#9025,
#9026,#9027,#9028,#9029),.UNSPECIFIED.,.F.,.F.,(4,1,1,1,1,1,1,4),(210.486707790516,
211.146280582813,212.143934878132,213.14158917345,214.139243468769,215.136897764087,
216.134552059406,216.769893097696),.UNSPECIFIED.);
#250=B_SPLINE_CURVE_WITH_KNOTS('',3,(#9030,#9031,#9032,#9033,#9034,#9035,
#9036,#9037,#9038,#9039),.UNSPECIFIED.,.F.,.F.,(4,1,1,1,1,1,1,4),(210.486707790516,
210.834408872398,211.832063167716,212.829717463035,213.827371758353,214.825026053672,
215.82268034899,216.769893097696),.UNSPECIFIED.);
#251=B_SPLINE_CURVE_WITH_KNOTS('',3,(#9044,#9045,#9046,#9047,#9048,#9049,
#9050,#9051,#9052,#9053),.UNSPECIFIED.,.F.,.F.,(4,1,1,1,1,1,1,4),(204.203522483337,
205.160354810902,206.158009106221,207.155663401539,208.153317696858,209.150971992176,
210.148626287495,210.486707790516),.UNSPECIFIED.);
#252=B_SPLINE_CURVE_WITH_KNOTS('',3,(#9054,#9055,#9056,#9057,#9058,#9059,
#9060,#9061,#9062,#9063),.UNSPECIFIED.,.F.,.F.,(4,1,1,1,1,1,1,4),(204.203522483337,
204.848483100487,205.846137395805,206.843791691124,207.841445986442,208.839100281761,
209.836754577079,210.486707790516),.UNSPECIFIED.);
#253=B_SPLINE_CURVE_WITH_KNOTS('',3,(#9068,#9069,#9070,#9071,#9072,#9073,
#9074,#9075,#9076,#9077,#9078),.UNSPECIFIED.,.F.,.F.,(4,1,1,1,1,1,1,1,4),
(197.920337176157,198.176774743672,199.174429038991,200.172083334309,201.169737629628,
202.167391924946,203.165046220265,204.162700515584,204.203522483337),
 .UNSPECIFIED.);
#254=B_SPLINE_CURVE_WITH_KNOTS('',3,(#9079,#9080,#9081,#9082,#9083,#9084,
#9085,#9086,#9087,#9088),.UNSPECIFIED.,.F.,.F.,(4,1,1,1,1,1,1,4),(197.920337176157,
198.862557328576,199.860211623894,200.857865919213,201.855520214531,202.85317450985,
203.850828805168,204.203522483337),.UNSPECIFIED.);
#255=B_SPLINE_CURVE_WITH_KNOTS('',3,(#9093,#9094,#9095,#9096,#9097,#9098,
#9099,#9100,#9101,#9102),.UNSPECIFIED.,.F.,.F.,(4,1,1,1,1,1,1,4),(191.637151868977,
192.190848971761,193.18850326708,194.186157562398,195.183811857717,196.181466153035,
197.179120448354,197.920337176157),.UNSPECIFIED.);
#256=B_SPLINE_CURVE_WITH_KNOTS('',3,(#9103,#9104,#9105,#9106,#9107,#9108,
#9109,#9110,#9111,#9112,#9113),.UNSPECIFIED.,.F.,.F.,(4,1,1,1,1,1,1,1,4),
(191.637151868977,191.878977261346,192.876631556665,193.874285851983,194.871940147302,
195.86959444262,196.867248737939,197.864903033257,197.920337176157),
 .UNSPECIFIED.);
#257=B_SPLINE_CURVE_WITH_KNOTS('',3,(#9118,#9119,#9120,#9121,#9122,#9123,
#9124,#9125,#9126,#9127),.UNSPECIFIED.,.F.,.F.,(4,1,1,1,1,1,1,4),(185.353966561798,
186.20492319985,187.202577495169,188.200231790487,189.197886085806,190.195540381124,
191.193194676443,191.637151868977),.UNSPECIFIED.);
#258=B_SPLINE_CURVE_WITH_KNOTS('',3,(#9128,#9129,#9130,#9131,#9132,#9133,
#9134,#9135,#9136,#9137),.UNSPECIFIED.,.F.,.F.,(4,1,1,1,1,1,1,4),(185.353966561798,
185.893051489435,186.890705784754,187.888360080072,188.886014375391,189.883668670709,
190.881322966028,191.637151868977),.UNSPECIFIED.);
#259=B_SPLINE_CURVE_WITH_KNOTS('',3,(#9142,#9143,#9144,#9145,#9146,#9147,
#9148,#9149,#9150,#9151,#9152),.UNSPECIFIED.,.F.,.F.,(4,1,1,1,1,1,1,1,4),
(179.070781254618,179.221343132621,180.218997427939,181.216651723258,182.214306018576,
183.211960313895,184.209614609213,185.207268904532,185.353966561798),
 .UNSPECIFIED.);
#260=B_SPLINE_CURVE_WITH_KNOTS('',3,(#9153,#9154,#9155,#9156,#9157,#9158,
#9159,#9160,#9161,#9162),.UNSPECIFIED.,.F.,.F.,(4,1,1,1,1,1,1,4),(179.070781254618,
179.907125717524,180.904780012842,181.902434308161,182.900088603479,183.897742898798,
184.895397194116,185.353966561798),.UNSPECIFIED.);
#261=B_SPLINE_CURVE_WITH_KNOTS('',3,(#9167,#9168,#9169,#9170,#9171,#9172,
#9173,#9174,#9175,#9176),.UNSPECIFIED.,.F.,.F.,(4,1,1,1,1,1,1,4),(172.787595947439,
173.23541736071,174.233071656028,175.230725951347,176.228380246665,177.226034541984,
178.223688837302,179.070781254618),.UNSPECIFIED.);
#262=B_SPLINE_CURVE_WITH_KNOTS('',3,(#9177,#9178,#9179,#9180,#9181,#9182,
#9183,#9184,#9185,#9186,#9187),.UNSPECIFIED.,.F.,.F.,(4,1,1,1,1,1,1,1,4),
(172.787595947439,172.923545650294,173.921199945613,174.918854240931,175.91650853625,
176.914162831568,177.911817126887,178.909471422205,179.070781254618),
 .UNSPECIFIED.);
#263=B_SPLINE_CURVE_WITH_KNOTS('',3,(#9192,#9193,#9194,#9195,#9196,#9197,
#9198,#9199,#9200,#9201),.UNSPECIFIED.,.F.,.F.,(4,1,1,1,1,1,1,4),(166.504410640259,
167.249491588799,168.247145884117,169.244800179436,170.242454474754,171.240108770073,
172.237763065391,172.787595947439),.UNSPECIFIED.);
#264=B_SPLINE_CURVE_WITH_KNOTS('',3,(#9202,#9203,#9204,#9205,#9206,#9207,
#9208,#9209,#9210,#9211),.UNSPECIFIED.,.F.,.F.,(4,1,1,1,1,1,1,4),(166.504410640259,
166.937619878383,167.935274173702,168.93292846902,169.930582764339,170.928237059657,
171.925891354976,172.787595947439),.UNSPECIFIED.);
#265=B_SPLINE_CURVE_WITH_KNOTS('',3,(#9216,#9217,#9218,#9219,#9220,#9221,
#9222,#9223,#9224,#9225,#9226),.UNSPECIFIED.,.F.,.F.,(4,1,1,1,1,1,1,1,4),
(160.22122533308,160.265911521569,161.263565816888,162.261220112206,163.258874407525,
164.256528702843,165.254182998162,166.25183729348,166.504410640259),
 .UNSPECIFIED.);
#266=B_SPLINE_CURVE_WITH_KNOTS('',3,(#9227,#9228,#9229,#9230,#9231,#9232,
#9233,#9234,#9235,#9236),.UNSPECIFIED.,.F.,.F.,(4,1,1,1,1,1,1,4),(160.22122533308,
160.951694106472,161.949348401791,162.947002697109,163.944656992428,164.942311287746,
165.939965583065,166.504410640259),.UNSPECIFIED.);
#267=B_SPLINE_CURVE_WITH_KNOTS('',3,(#9241,#9242,#9243,#9244,#9245,#9246,
#9247,#9248,#9249,#9250),.UNSPECIFIED.,.F.,.F.,(4,1,1,1,1,1,1,4),(153.9380400259,
154.279985749658,155.277640044976,156.275294340295,157.272948635613,158.270602930932,
159.268257226251,160.22122533308),.UNSPECIFIED.);
#268=B_SPLINE_CURVE_WITH_KNOTS('',3,(#9251,#9252,#9253,#9254,#9255,#9256,
#9257,#9258,#9259,#9260,#9261),.UNSPECIFIED.,.F.,.F.,(4,1,1,1,1,1,1,1,4),
(153.9380400259,153.968114039243,154.965768334561,155.96342262988,156.961076925198,
157.958731220517,158.956385515835,159.954039811154,160.22122533308),
 .UNSPECIFIED.);
#269=B_SPLINE_CURVE_WITH_KNOTS('',3,(#9266,#9267,#9268,#9269,#9270,#9271,
#9272,#9273,#9274,#9275),.UNSPECIFIED.,.F.,.F.,(4,1,1,1,1,1,1,4),(147.65485471872,
148.294059977747,149.291714273065,150.289368568384,151.287022863702,152.284677159021,
153.282331454339,153.9380400259),.UNSPECIFIED.);
#270=B_SPLINE_CURVE_WITH_KNOTS('',3,(#9276,#9277,#9278,#9279,#9280,#9281,
#9282,#9283,#9284,#9285),.UNSPECIFIED.,.F.,.F.,(4,1,1,1,1,1,1,4),(147.654854718721,
147.982188267332,148.97984256265,149.977496857969,150.975151153287,151.972805448606,
152.970459743924,153.9380400259),.UNSPECIFIED.);
#271=B_SPLINE_CURVE_WITH_KNOTS('',3,(#9290,#9291,#9292,#9293,#9294,#9295,
#9296,#9297,#9298,#9299),.UNSPECIFIED.,.F.,.F.,(4,1,1,1,1,1,1,4),(141.371669411541,
142.308134205836,143.305788501154,144.303442796473,145.301097091791,146.29875138711,
147.296405682428,147.65485471872),.UNSPECIFIED.);
#272=B_SPLINE_CURVE_WITH_KNOTS('',3,(#9300,#9301,#9302,#9303,#9304,#9305,
#9306,#9307,#9308,#9309),.UNSPECIFIED.,.F.,.F.,(4,1,1,1,1,1,1,4),(141.371669411541,
141.99626249542,142.993916790739,143.991571086058,144.989225381376,145.986879676695,
146.984533972013,147.654854718721),.UNSPECIFIED.);
#273=B_SPLINE_CURVE_WITH_KNOTS('',3,(#9314,#9315,#9316,#9317,#9318,#9319,
#9320,#9321,#9322,#9323,#9324),.UNSPECIFIED.,.F.,.F.,(4,1,1,1,1,1,1,1,4),
(135.088484104361,135.324554138606,136.322208433925,137.319862729243,138.317517024562,
139.31517131988,140.312825615199,141.310479910517,141.371669411541),
 .UNSPECIFIED.);
#274=B_SPLINE_CURVE_WITH_KNOTS('',3,(#9325,#9326,#9327,#9328,#9329,#9330,
#9331,#9332,#9333,#9334),.UNSPECIFIED.,.F.,.F.,(4,1,1,1,1,1,1,4),(135.088484104361,
136.010336723509,137.007991018828,138.005645314146,139.003299609465,140.000953904783,
140.998608200102,141.371669411541),.UNSPECIFIED.);
#275=B_SPLINE_CURVE_WITH_KNOTS('',3,(#9339,#9340,#9341,#9342,#9343,#9344,
#9345,#9346,#9347,#9348),.UNSPECIFIED.,.F.,.F.,(4,1,1,1,1,1,1,4),(128.805298797182,
129.338628366695,130.336282662014,131.333936957332,132.331591252651,133.329245547969,
134.326899843288,135.088484104361),.UNSPECIFIED.);
#276=B_SPLINE_CURVE_WITH_KNOTS('',3,(#9349,#9350,#9351,#9352,#9353,#9354,
#9355,#9356,#9357,#9358,#9359),.UNSPECIFIED.,.F.,.F.,(4,1,1,1,1,1,1,1,4),
(128.805298797182,129.02675665628,130.024410951598,131.022065246917,132.019719542235,
133.017373837554,134.015028132872,135.012682428191,135.088484104361),
 .UNSPECIFIED.);
#277=B_SPLINE_CURVE_WITH_KNOTS('',3,(#9364,#9365,#9366,#9367,#9368,#9369,
#9370,#9371,#9372,#9373),.UNSPECIFIED.,.F.,.F.,(4,1,1,1,1,1,1,4),(122.522113490002,
123.352702594784,124.350356890103,125.348011185421,126.34566548074,127.343319776058,
128.340974071377,128.805298797182),.UNSPECIFIED.);
#278=B_SPLINE_CURVE_WITH_KNOTS('',3,(#9374,#9375,#9376,#9377,#9378,#9379,
#9380,#9381,#9382,#9383),.UNSPECIFIED.,.F.,.F.,(4,1,1,1,1,1,1,4),(122.522113490002,
123.040830884369,124.038485179687,125.036139475006,126.033793770324,127.031448065643,
128.029102360961,128.805298797182),.UNSPECIFIED.);
#279=B_SPLINE_CURVE_WITH_KNOTS('',3,(#9388,#9389,#9390,#9391,#9392,#9393,
#9394,#9395,#9396,#9397,#9398),.UNSPECIFIED.,.F.,.F.,(4,1,1,1,1,1,1,1,4),
(116.238928182823,116.369122527555,117.366776822873,118.364431118192,119.36208541351,
120.359739708829,121.357394004147,122.355048299466,122.522113490002),
 .UNSPECIFIED.);
#280=B_SPLINE_CURVE_WITH_KNOTS('',3,(#9399,#9400,#9401,#9402,#9403,#9404,
#9405,#9406,#9407,#9408),.UNSPECIFIED.,.F.,.F.,(4,1,1,1,1,1,1,4),(116.238928182823,
117.054905112458,118.052559407776,119.050213703095,120.047867998413,121.045522293732,
122.04317658905,122.522113490002),.UNSPECIFIED.);
#281=B_SPLINE_CURVE_WITH_KNOTS('',3,(#9413,#9414,#9415,#9416,#9417,#9418,
#9419,#9420,#9421,#9422),.UNSPECIFIED.,.F.,.F.,(4,1,1,1,1,1,1,4),(109.955742875643,
110.383196755643,111.380851050962,112.37850534628,113.376159641599,114.373813936918,
115.371468232236,116.238928182823),.UNSPECIFIED.);
#282=B_SPLINE_CURVE_WITH_KNOTS('',3,(#9423,#9424,#9425,#9426,#9427,#9428,
#9429,#9430,#9431,#9432,#9433),.UNSPECIFIED.,.F.,.F.,(4,1,1,1,1,1,1,1,4),
(109.955742875643,110.071325045228,111.068979340547,112.066633635865,113.064287931184,
114.061942226502,115.059596521821,116.057250817139,116.238928182823),
 .UNSPECIFIED.);
#283=B_SPLINE_CURVE_WITH_KNOTS('',3,(#9438,#9439,#9440,#9441,#9442,#9443,
#9444,#9445,#9446,#9447),.UNSPECIFIED.,.F.,.F.,(4,1,1,1,1,1,1,4),(103.672557568463,
104.397270983732,105.394925279051,106.392579574369,107.390233869688,108.387888165006,
109.385542460325,109.955742875643),.UNSPECIFIED.);
#284=B_SPLINE_CURVE_WITH_KNOTS('',3,(#9448,#9449,#9450,#9451,#9452,#9453,
#9454,#9455,#9456,#9457),.UNSPECIFIED.,.F.,.F.,(4,1,1,1,1,1,1,4),(103.672557568463,
104.085399273317,105.083053568636,106.080707863954,107.078362159273,108.076016454591,
109.07367074991,109.955742875643),.UNSPECIFIED.);
#285=B_SPLINE_CURVE_WITH_KNOTS('',3,(#9462,#9463,#9464,#9465,#9466,#9467,
#9468,#9469,#9470,#9471,#9472),.UNSPECIFIED.,.F.,.F.,(4,1,1,1,1,1,1,1,4),
(97.3893722612838,97.4136909165028,98.4113452118213,99.4089995071398,100.406653802458,
101.404308097777,102.401962393095,103.399616688414,103.672557568463),
 .UNSPECIFIED.);
#286=B_SPLINE_CURVE_WITH_KNOTS('',3,(#9473,#9474,#9475,#9476,#9477,#9478,
#9479,#9480,#9481,#9482),.UNSPECIFIED.,.F.,.F.,(4,1,1,1,1,1,1,4),(97.3893722612839,
98.099473501406,99.0971277967245,100.094782092043,101.092436387362,102.09009068268,
103.087744977999,103.672557568463),.UNSPECIFIED.);
#287=B_SPLINE_CURVE_WITH_KNOTS('',3,(#9487,#9488,#9489,#9490,#9491,#9492,
#9493,#9494,#9495,#9496),.UNSPECIFIED.,.F.,.F.,(4,1,1,1,1,1,1,4),(91.1061869541042,
91.4277651445918,92.4254194399103,93.4230737352288,94.4207280305473,95.4183823258658,
96.4160366211843,97.3893722612838),.UNSPECIFIED.);
#288=B_SPLINE_CURVE_WITH_KNOTS('',3,(#9497,#9498,#9499,#9500,#9501,#9502,
#9503,#9504,#9505,#9506,#9507),.UNSPECIFIED.,.F.,.F.,(4,1,1,1,1,1,1,1,4),
(91.1061869541043,91.1158934341764,92.1135477294949,93.1112020248134,94.1088563201319,
95.1065106154505,96.104164910769,97.1018192060875,97.3893722612839),
 .UNSPECIFIED.);
#289=B_SPLINE_CURVE_WITH_KNOTS('',3,(#9512,#9513,#9514,#9515,#9516,#9517,
#9518,#9519,#9520,#9521),.UNSPECIFIED.,.F.,.F.,(4,1,1,1,1,1,1,4),(84.8230016469246,
85.4418393726807,86.4394936679992,87.4371479633177,88.4348022586362,89.4324565539547,
90.4301108492732,91.1061869541042),.UNSPECIFIED.);
#290=B_SPLINE_CURVE_WITH_KNOTS('',3,(#9522,#9523,#9524,#9525,#9526,#9527,
#9528,#9529,#9530,#9531),.UNSPECIFIED.,.F.,.F.,(4,1,1,1,1,1,1,4),(84.8230016469247,
85.1299676622653,86.1276219575839,87.1252762529024,88.1229305482209,89.1205848435394,
90.1182391388579,91.1061869541043),.UNSPECIFIED.);
#291=B_SPLINE_CURVE_WITH_KNOTS('',3,(#9536,#9537,#9538,#9539,#9540,#9541,
#9542,#9543,#9544,#9545),.UNSPECIFIED.,.F.,.F.,(4,1,1,1,1,1,1,4),(78.539816339745,
79.4559136007696,80.4535678960881,81.4512221914066,82.4488764867252,83.4465307820437,
84.4441850773622,84.8230016469246),.UNSPECIFIED.);
#292=B_SPLINE_CURVE_WITH_KNOTS('',3,(#9546,#9547,#9548,#9549,#9550,#9551,
#9552,#9553,#9554,#9555),.UNSPECIFIED.,.F.,.F.,(4,1,1,1,1,1,1,4),(78.5398163397451,
79.1440418903543,80.1416961856728,81.1393504809913,82.1370047763098,83.1346590716283,
84.1323133669468,84.8230016469247),.UNSPECIFIED.);
#293=B_SPLINE_CURVE_WITH_KNOTS('',3,(#9560,#9561,#9562,#9563,#9564,#9565,
#9566,#9567,#9568,#9569,#9570),.UNSPECIFIED.,.F.,.F.,(4,1,1,1,1,1,1,1,4),
(72.2566310325654,72.4723335335401,73.4699878288586,74.4676421241771,75.4652964194956,
76.4629507148141,77.4606050101326,78.4582593054511,78.539816339745),
 .UNSPECIFIED.);
#294=B_SPLINE_CURVE_WITH_KNOTS('',3,(#9571,#9572,#9573,#9574,#9575,#9576,
#9577,#9578,#9579,#9580),.UNSPECIFIED.,.F.,.F.,(4,1,1,1,1,1,1,4),(72.2566310325655,
73.1581161184432,74.1557704137617,75.1534247090802,76.1510790043987,77.1487332997173,
78.1463875950358,78.5398163397451),.UNSPECIFIED.);
#295=B_SPLINE_CURVE_WITH_KNOTS('',3,(#9585,#9586,#9587,#9588,#9589,#9590,
#9591,#9592,#9593,#9594),.UNSPECIFIED.,.F.,.F.,(4,1,1,1,1,1,1,4),(65.9734457253858,
66.486407761629,67.4840620569475,68.481716352266,69.4793706475845,70.477024942903,
71.4746792382215,72.2566310325654),.UNSPECIFIED.);
#296=B_SPLINE_CURVE_WITH_KNOTS('',3,(#9595,#9596,#9597,#9598,#9599,#9600,
#9601,#9602,#9603,#9604,#9605),.UNSPECIFIED.,.F.,.F.,(4,1,1,1,1,1,1,1,4),
(65.9734457253859,66.1745360512136,67.1721903465321,68.1698446418506,69.1674989371692,
70.1651532324877,71.1628075278062,72.1604618231247,72.2566310325655),
 .UNSPECIFIED.);
#297=B_SPLINE_CURVE_WITH_KNOTS('',3,(#9610,#9611,#9612,#9613,#9614,#9615,
#9616,#9617,#9618,#9619),.UNSPECIFIED.,.F.,.F.,(4,1,1,1,1,1,1,4),(59.6902604182063,
60.5004819897179,61.4981362850364,62.4957905803549,63.4934448756734,64.491099170992,
65.4887534663105,65.9734457253858),.UNSPECIFIED.);
#298=B_SPLINE_CURVE_WITH_KNOTS('',3,(#9620,#9621,#9622,#9623,#9624,#9625,
#9626,#9627,#9628,#9629),.UNSPECIFIED.,.F.,.F.,(4,1,1,1,1,1,1,4),(59.6902604182063,
60.1886102793026,61.1862645746211,62.1839188699396,63.1815731652581,64.1792274605766,
65.1768817558951,65.9734457253859),.UNSPECIFIED.);
#299=B_SPLINE_CURVE_WITH_KNOTS('',3,(#9634,#9635,#9636,#9637,#9638,#9639,
#9640,#9641,#9642,#9643,#9644),.UNSPECIFIED.,.F.,.F.,(4,1,1,1,1,1,1,1,4),
(53.4070751110267,53.5169019224883,54.5145562178069,55.5122105131254,56.5098648084439,
57.5075191037624,58.5051733990809,59.5028276943994,59.6902604182063),
 .UNSPECIFIED.);
#300=B_SPLINE_CURVE_WITH_KNOTS('',3,(#9645,#9646,#9647,#9648,#9649,#9650,
#9651,#9652,#9653,#9654),.UNSPECIFIED.,.F.,.F.,(4,1,1,1,1,1,1,4),(53.4070751110267,
54.2026845073915,55.20033880271,56.1979930980285,57.195647393347,58.1933016886655,
59.190955983984,59.6902604182063),.UNSPECIFIED.);
#301=B_SPLINE_CURVE_WITH_KNOTS('',3,(#9659,#9660,#9661,#9662,#9663,#9664,
#9665,#9666,#9667,#9668),.UNSPECIFIED.,.F.,.F.,(4,1,1,1,1,1,1,4),(47.1238898038471,
47.5309761505773,48.5286304458958,49.5262847412143,50.5239390365328,51.5215933318513,
52.5192476271698,53.4070751110267),.UNSPECIFIED.);
#302=B_SPLINE_CURVE_WITH_KNOTS('',3,(#9669,#9670,#9671,#9672,#9673,#9674,
#9675,#9676,#9677,#9678,#9679),.UNSPECIFIED.,.F.,.F.,(4,1,1,1,1,1,1,1,4),
(47.1238898038471,47.2191044401619,48.2167587354804,49.2144130307989,50.2120673261174,
51.209721621436,52.2073759167545,53.205030212073,53.4070751110267),
 .UNSPECIFIED.);
#303=B_SPLINE_CURVE_WITH_KNOTS('',3,(#9684,#9685,#9686,#9687,#9688,#9689,
#9690,#9691,#9692,#9693),.UNSPECIFIED.,.F.,.F.,(4,1,1,1,1,1,1,4),(40.8407044966675,
41.5450503786662,42.5427046739847,43.5403589693032,44.5380132646217,45.5356675599403,
46.5333218552588,47.1238898038471),.UNSPECIFIED.);
#304=B_SPLINE_CURVE_WITH_KNOTS('',3,(#9694,#9695,#9696,#9697,#9698,#9699,
#9700,#9701,#9702,#9703),.UNSPECIFIED.,.F.,.F.,(4,1,1,1,1,1,1,4),(40.8407044966675,
41.2331786682508,42.2308329635693,43.2284872588879,44.2261415542064,45.2237958495249,
46.2214501448434,47.1238898038471),.UNSPECIFIED.);
#305=B_SPLINE_CURVE_WITH_KNOTS('',3,(#9708,#9709,#9710,#9711,#9712,#9713,
#9714,#9715,#9716,#9717,#9718),.UNSPECIFIED.,.F.,.F.,(4,1,1,1,1,1,1,1,4),
(34.5575191894879,34.5614703114366,35.5591246067551,36.5567789020737,37.5544331973922,
38.5520874927107,39.5497417880292,40.5473960833477,40.8407044966675),
 .UNSPECIFIED.);
#306=B_SPLINE_CURVE_WITH_KNOTS('',3,(#9719,#9720,#9721,#9722,#9723,#9724,
#9725,#9726,#9727,#9728),.UNSPECIFIED.,.F.,.F.,(4,1,1,1,1,1,1,4),(34.5575191894879,
35.2472528963398,36.2449071916583,37.2425614869768,38.2402157822953,39.2378700776138,
40.2355243729323,40.8407044966675),.UNSPECIFIED.);
#307=B_SPLINE_CURVE_WITH_KNOTS('',3,(#9733,#9734,#9735,#9736,#9737,#9738,
#9739,#9740,#9741,#9742),.UNSPECIFIED.,.F.,.F.,(4,1,1,1,1,1,1,4),(28.2743338823083,
28.5755445395256,29.5731988348441,30.5708531301626,31.5685074254811,32.5661617207996,
33.5638160161181,34.5575191894879),.UNSPECIFIED.);
#308=B_SPLINE_CURVE_WITH_KNOTS('',3,(#9743,#9744,#9745,#9746,#9747,#9748,
#9749,#9750,#9751,#9752),.UNSPECIFIED.,.F.,.F.,(4,1,1,1,1,1,1,4),(28.2743338823084,
29.2613271244287,30.2589814197472,31.2566357150657,32.2542900103842,33.2519443057027,
34.2495986010213,34.5575191894879),.UNSPECIFIED.);
#309=B_SPLINE_CURVE_WITH_KNOTS('',3,(#9757,#9758,#9759,#9760,#9761,#9762,
#9763,#9764,#9765,#9766),.UNSPECIFIED.,.F.,.F.,(4,1,1,1,1,1,1,4),(21.9911485751287,
22.5896187676145,23.587273062933,24.5849273582515,25.58258165357,26.5802359488886,
27.5778902442071,28.2743338823083),.UNSPECIFIED.);
#310=B_SPLINE_CURVE_WITH_KNOTS('',3,(#9767,#9768,#9769,#9770,#9771,#9772,
#9773,#9774,#9775,#9776,#9777),.UNSPECIFIED.,.F.,.F.,(4,1,1,1,1,1,1,1,4),
(21.9911485751288,22.2777470571991,23.2754013525176,24.2730556478361,25.2707099431546,
26.2683642384732,27.2660185337917,28.2636728291102,28.2743338823084),
 .UNSPECIFIED.);
#311=B_SPLINE_CURVE_WITH_KNOTS('',3,(#9782,#9783,#9784,#9785,#9786,#9787,
#9788,#9789,#9790,#9791),.UNSPECIFIED.,.F.,.F.,(4,1,1,1,1,1,1,4),(15.7079632679491,
16.6036929957034,17.601347291022,18.5990015863405,19.596655881659,20.5943101769775,
21.591964472296,21.9911485751287),.UNSPECIFIED.);
#312=B_SPLINE_CURVE_WITH_KNOTS('',3,(#9792,#9793,#9794,#9795,#9796,#9797,
#9798,#9799,#9800,#9801),.UNSPECIFIED.,.F.,.F.,(4,1,1,1,1,1,1,4),(15.7079632679492,
16.291821285288,17.2894755806066,18.2871298759251,19.2847841712436,20.2824384665621,
21.2800927618806,21.9911485751288),.UNSPECIFIED.);
#313=B_SPLINE_CURVE_WITH_KNOTS('',3,(#10687,#10688,#10689,#10690,#10691,
#10692,#10693,#10694,#10695,#10696,#10697,#10698,#10699,#10700,#10701,#10702,
#10703,#10704,#10705,#10706,#10707,#10708,#10709,#10710,#10711,#10712,#10713,
#10714,#10715,#10716,#10717,#10718,#10719,#10720,#10721,#10722,#10723,#10724,
#10725,#10726,#10727,#10728,#10729,#10730,#10731,#10732,#10733,#10734,#10735,
#10736,#10737,#10738,#10739,#10740,#10741),.UNSPECIFIED.,.F.,.F.,(4,3,3,
3,3,3,3,3,3,3,3,3,3,3,3,3,3,3,4),(0.,0.0136872263540572,0.0521656178595838,
0.0709950800646878,0.0819953190919729,0.119249023879074,0.145058748625905,
0.157048448925498,0.192145397802465,0.199552864933563,0.212199804588965,
0.222691438606214,0.258617973706117,0.274171447851467,0.289117136857619,
0.312609296851327,0.324805558922168,0.357088803957493,0.366397579005826),
 .UNSPECIFIED.);
#314=B_SPLINE_CURVE_WITH_KNOTS('',3,(#10742,#10743,#10744,#10745),
 .UNSPECIFIED.,.F.,.F.,(4,4),(214.742491482136,215.423496246157),
 .UNSPECIFIED.);
#315=B_SPLINE_CURVE_WITH_KNOTS('',3,(#10747,#10748,#10749,#10750,#10751,
#10752,#10753,#10754,#10755,#10756,#10757,#10758,#10759,#10760,#10761,#10762,
#10763,#10764,#10765,#10766,#10767,#10768,#10769,#10770,#10771,#10772,#10773,
#10774,#10775,#10776,#10777,#10778,#10779,#10780,#10781,#10782,#10783,#10784,
#10785,#10786,#10787,#10788,#10789,#10790,#10791,#10792,#10793,#10794,#10795,
#10796,#10797,#10798),.UNSPECIFIED.,.F.,.F.,(4,3,3,3,3,3,3,3,3,3,3,3,3,
3,3,3,3,4),(-0.366397579005832,-0.355349081053819,-0.328627709487849,-0.316006317805062,
-0.292294699921123,-0.280145524705702,-0.245167839456388,-0.218343989495843,
-0.207795842608001,-0.187146499846321,-0.163753187365531,-0.149466290679141,
-0.138688713158187,-0.10401653486864,-0.0826655685122029,-0.0667932349897769,
-0.0282993460444213,0.),.UNSPECIFIED.);
#316=B_SPLINE_CURVE_WITH_KNOTS('',3,(#10799,#10800,#10801,#10802,#10803,
#10804,#10805,#10806,#10807),.UNSPECIFIED.,.F.,.F.,(4,1,1,1,1,1,4),(10.3757270560181,
11.3035498086955,12.301204104014,13.2988583993325,14.296512694651,15.2941669899695,
15.7079632679492),.UNSPECIFIED.);
#317=B_SPLINE_CURVE_WITH_KNOTS('',3,(#10811,#10812,#10813,#10814,#10815,
#10816,#10817,#10818),.UNSPECIFIED.,.F.,.F.,(4,1,1,1,1,4),(11.6154215191109,
12.6130758144294,13.6107301097479,14.6083844050664,15.6060387003849,15.7079632679491),
 .UNSPECIFIED.);
#318=B_SPLINE_CURVE_WITH_KNOTS('',3,(#11703,#11704,#11705,#11706,#11707,
#11708,#11709,#11710,#11711,#11712,#11713,#11714,#11715,#11716,#11717,#11718,
#11719,#11720,#11721,#11722,#11723,#11724,#11725,#11726,#11727,#11728,#11729,
#11730,#11731,#11732,#11733,#11734,#11735,#11736,#11737,#11738,#11739,#11740,
#11741,#11742,#11743,#11744,#11745,#11746,#11747,#11748,#11749,#11750,#11751,
#11752,#11753,#11754,#11755,#11756,#11757),.UNSPECIFIED.,.F.,.F.,(4,3,3,
3,3,3,3,3,3,3,3,3,3,3,3,3,3,3,4),(0.,0.0110072508574968,0.0432941145547806,
0.0597161191659724,0.0689602245586863,0.103423950716991,0.120946125282339,
0.133710039597458,0.169449851669546,0.178576016460901,0.192751466168984,
0.204131677343237,0.24002978635429,0.257655102053338,0.272192488363931,
0.297601230030268,0.313197869948207,0.326770085092486,0.364629307890676),
 .UNSPECIFIED.);
#319=B_SPLINE_CURVE_WITH_KNOTS('',3,(#11758,#11759,#11760,#11761,#11762,
#11763,#11764,#11765,#11766,#11767,#11768,#11769,#11770,#11771,#11772,#11773,
#11774,#11775,#11776,#11777,#11778,#11779,#11780,#11781,#11782,#11783,#11784,
#11785,#11786,#11787,#11788,#11789,#11790,#11791,#11792,#11793,#11794,#11795,
#11796,#11797,#11798,#11799,#11800,#11801,#11802,#11803,#11804,#11805,#11806,
#11807,#11808,#11809,#11810,#11811,#11812),.UNSPECIFIED.,.F.,.F.,(4,3,3,
3,3,3,3,3,3,3,3,3,3,3,3,3,3,3,4),(-0.364629307890679,-0.351009649103909,
-0.324517397172783,-0.304129683158625,-0.282910327436154,-0.263912543184838,
-0.252746321376793,-0.216330856983722,-0.197981750539286,-0.186600442527354,
-0.166229720628164,-0.130494010253894,-0.119373904450406,-0.0895304283378048,
-0.0729804099452609,-0.062655130809591,-0.0518856098027967,-0.0196333504494857,
0.),.UNSPECIFIED.);
#320=B_SPLINE_CURVE_WITH_KNOTS('',3,(#11868,#11869,#11870,#11871),
 .UNSPECIFIED.,.F.,.F.,(4,4),(-35.9039160410262,-35.2623097995902),
 .UNSPECIFIED.);
#321=B_SPLINE_CURVE_WITH_KNOTS('',3,(#11877,#11878,#11879,#11880,#11881,
#11882,#11883,#11884,#11885,#11886,#11887,#11888,#11889,#11890,#11891,#11892,
#11893,#11894,#11895),.UNSPECIFIED.,.F.,.F.,(4,3,3,3,3,3,4),(32.7257487910699,
32.9292487870506,33.9271048109006,34.9249608347506,35.9228168586006,36.9206728824506,
37.9185289063006),.UNSPECIFIED.);
#322=B_SPLINE_CURVE_WITH_KNOTS('',3,(#11897,#11898,#11899,#11900,#11901,
#11902,#11903,#11904,#11905,#11906,#11907,#11908,#11909,#11910,#11911,#11912,
#11913,#11914,#11915,#11916,#11917,#11918),.UNSPECIFIED.,.F.,.F.,(4,3,3,
3,3,3,3,4),(-35.2623097995902,-34.9249608347506,-33.9271048109006,-32.9292487870506,
-31.9313927632006,-30.9335367393505,-29.9356807155005,-28.9791244924106),
 .UNSPECIFIED.);
#323=B_SPLINE_CURVE_WITH_KNOTS('',3,(#11923,#11924,#11925,#11926,#11927,
#11928,#11929,#11930,#11931,#11932,#11933,#11934,#11935,#11936,#11937,#11938,
#11939,#11940,#11941,#11942,#11943,#11944),.UNSPECIFIED.,.F.,.F.,(4,3,3,
3,3,3,3,4),(26.4425634838903,26.9421126439505,27.9399686678005,28.9378246916505,
29.9356807155005,30.9335367393505,31.9313927632005,32.7257487910699),
 .UNSPECIFIED.);
#324=B_SPLINE_CURVE_WITH_KNOTS('',3,(#11945,#11946,#11947,#11948,#11949,
#11950,#11951,#11952,#11953,#11954,#11955,#11956,#11957,#11958,#11959,#11960,
#11961,#11962,#11963,#11964,#11965,#11966,#11967,#11968,#11969),
 .UNSPECIFIED.,.F.,.F.,(4,3,3,3,3,3,3,3,4),(-28.9791244924106,-28.9378246916505,
-27.9399686678005,-26.9421126439505,-25.9442566201005,-24.9464005962504,
-23.9485445724004,-22.9506885485504,-22.695939185231),.UNSPECIFIED.);
#325=B_SPLINE_CURVE_WITH_KNOTS('',3,(#11974,#11975,#11976,#11977,#11978,
#11979,#11980,#11981,#11982,#11983,#11984,#11985,#11986,#11987,#11988,#11989,
#11990,#11991,#11992,#11993,#11994,#11995),.UNSPECIFIED.,.F.,.F.,(4,3,3,
3,3,3,3,4),(20.1593781767107,20.9549765008504,21.9528325247004,22.9506885485504,
23.9485445724004,24.9464005962504,25.9442566201004,26.4425634838903),
 .UNSPECIFIED.);
#326=B_SPLINE_CURVE_WITH_KNOTS('',3,(#11996,#11997,#11998,#11999,#12000,
#12001,#12002,#12003,#12004,#12005,#12006,#12007,#12008,#12009,#12010,#12011,
#12012,#12013,#12014,#12015,#12016,#12017),.UNSPECIFIED.,.F.,.F.,(4,3,3,
3,3,3,3,4),(-22.695939185231,-21.9528325247004,-20.9549765008504,-19.9571204770003,
-18.9592644531503,-17.9614084293003,-16.9635524054503,-16.4127538780514),
 .UNSPECIFIED.);
#327=B_SPLINE_CURVE_WITH_KNOTS('',3,(#12022,#12023,#12024,#12025,#12026,
#12027,#12028,#12029,#12030,#12031,#12032,#12033,#12034,#12035,#12036,#12037,
#12038,#12039,#12040,#12041,#12042,#12043,#12044,#12045,#12046),
 .UNSPECIFIED.,.F.,.F.,(4,3,3,3,3,3,3,3,4),(13.8761928695312,13.9699843339002,
14.9678403577503,15.9656963816003,16.9635524054503,17.9614084293003,18.9592644531503,
19.9571204770003,20.1593781767107),.UNSPECIFIED.);
#328=B_SPLINE_CURVE_WITH_KNOTS('',3,(#12047,#12048,#12049,#12050,#12051,
#12052,#12053,#12054,#12055,#12056,#12057,#12058,#12059,#12060,#12061,#12062,
#12063,#12064,#12065,#12066,#12067,#12068),.UNSPECIFIED.,.F.,.F.,(4,3,3,
3,3,3,3,4),(-16.4127538780514,-15.9656963816003,-14.9678403577503,-13.9699843339002,
-12.9721283100502,-11.9742722862002,-10.9764162623502,-10.1295685708718),
 .UNSPECIFIED.);
#329=B_SPLINE_CURVE_WITH_KNOTS('',3,(#12074,#12075,#12076,#12077,#12078,
#12079,#12080,#12081,#12082,#12083,#12084,#12085,#12086),.UNSPECIFIED.,
 .F.,.F.,(4,3,3,3,4),(-3.84638326369223,-2.99356807155005,-1.99571204770004,
-0.99785602385002,0.),.UNSPECIFIED.);
#330=B_SPLINE_CURVE_WITH_KNOTS('',3,(#12089,#12090,#12091,#12092,#12093,
#12094,#12095,#12096,#12097,#12098,#12099,#12100,#12101,#12102,#12103,#12104,
#12105,#12106,#12107),.UNSPECIFIED.,.F.,.F.,(4,3,3,3,3,3,4),(2.01461286527443,
2.99356807155005,3.99142409540007,4.98928011925009,5.9871361431001,6.98499216695013,
7.59300756235157),.UNSPECIFIED.);
#331=B_SPLINE_CURVE_WITH_KNOTS('',3,(#12113,#12114,#12115,#12116,#12117,
#12118),.UNSPECIFIED.,.F.,.F.,(4,1,1,4),(47.1238898038469,47.7843968628573,
48.7822528867074,49.7801089105574),.UNSPECIFIED.);
#332=B_SPLINE_CURVE_WITH_KNOTS('',3,(#12121,#12122,#12123,#12124,#12125,
#12126,#12127),.UNSPECIFIED.,.F.,.F.,(4,1,1,1,4),(47.1238898038469,47.3273897998275,
48.3252458236776,49.3231018475276,50.3020570538032),.UNSPECIFIED.);
#333=B_SPLINE_CURVE_WITH_KNOTS('',3,(#12132,#12133,#12134,#12135,#12136,
#12137,#12138,#12139,#12140,#12141),.UNSPECIFIED.,.F.,.F.,(4,1,1,1,1,1,
1,4),(40.8407044966673,41.7972607197572,42.7951167436073,43.7929727674573,
44.7908287913073,45.7886848151573,46.7865408390073,47.1238898038469),
 .UNSPECIFIED.);
#334=B_SPLINE_CURVE_WITH_KNOTS('',3,(#12142,#12143,#12144,#12145,#12146,
#12147,#12148,#12149,#12150,#12151),.UNSPECIFIED.,.F.,.F.,(4,1,1,1,1,1,
1,4),(40.8407044966673,41.3402536567274,42.3381096805775,43.3359657044275,
44.3338217282775,45.3316777521275,46.3295337759775,47.1238898038469),
 .UNSPECIFIED.);
#335=B_SPLINE_CURVE_WITH_KNOTS('',3,(#12156,#12157,#12158,#12159,#12160,
#12161,#12162,#12163,#12164,#12165,#12166),.UNSPECIFIED.,.F.,.F.,(4,1,1,
1,1,1,1,1,4),(34.5575191894877,34.8122685528071,35.8101245766571,36.8079806005072,
37.8058366243572,38.8036926482072,39.8015486720572,40.7994046959072,40.8407044966673),
 .UNSPECIFIED.);
#336=B_SPLINE_CURVE_WITH_KNOTS('',3,(#12167,#12168,#12169,#12170,#12171,
#12172,#12173,#12174,#12175,#12176),.UNSPECIFIED.,.F.,.F.,(4,1,1,1,1,1,
1,4),(34.5575191894877,35.3531175136273,36.3509735374774,37.3488295613274,
38.3466855851774,39.3445416090274,40.3423976328774,40.8407044966673),
 .UNSPECIFIED.);
#337=B_SPLINE_CURVE_WITH_KNOTS('',3,(#12181,#12182,#12183,#12184,#12185,
#12186,#12187,#12188,#12189,#12190),.UNSPECIFIED.,.F.,.F.,(4,1,1,1,1,1,
1,4),(28.2743338823081,28.825132409707,29.822988433557,30.8208444574071,
31.8187004812571,32.8165565051071,33.8144125289571,34.5575191894877),
 .UNSPECIFIED.);
#338=B_SPLINE_CURVE_WITH_KNOTS('',3,(#12191,#12192,#12193,#12194,#12195,
#12196,#12197,#12198,#12199,#12200,#12201),.UNSPECIFIED.,.F.,.F.,(4,1,1,
1,1,1,1,1,4),(28.2743338823081,28.3681253466772,29.3659813705272,30.3638373943772,
31.3616934182273,32.3595494420773,33.3574054659273,34.3552614897773,34.5575191894877),
 .UNSPECIFIED.);
#339=B_SPLINE_CURVE_WITH_KNOTS('',3,(#12206,#12207,#12208,#12209,#12210,
#12211,#12212,#12213,#12214,#12215),.UNSPECIFIED.,.F.,.F.,(4,1,1,1,1,1,
1,4),(21.9911485751285,22.8379962666069,23.8358522904569,24.833708314307,
25.831564338157,26.829420362007,27.827276385857,28.2743338823081),
 .UNSPECIFIED.);
#340=B_SPLINE_CURVE_WITH_KNOTS('',3,(#12216,#12217,#12218,#12219,#12220,
#12221,#12222,#12223,#12224,#12225),.UNSPECIFIED.,.F.,.F.,(4,1,1,1,1,1,
1,4),(21.9911485751285,22.3809892035771,23.3788452274271,24.3767012512771,
25.3745572751272,26.3724132989772,27.3702693228272,28.2743338823081),
 .UNSPECIFIED.);
#341=B_SPLINE_CURVE_WITH_KNOTS('',3,(#12231,#12232,#12233,#12234,#12235),
 .UNSPECIFIED.,.F.,.F.,(4,1,4),(14.398141012777,15.395997036627,15.7079632679489),
 .UNSPECIFIED.);
#342=B_SPLINE_CURVE_WITH_KNOTS('',3,(#12238,#12239,#12240,#12241,#12242),
 .UNSPECIFIED.,.F.,.F.,(4,1,4),(13.8761928695312,14.8551480758068,15.7079632679489),
 .UNSPECIFIED.);
#343=B_SPLINE_CURVE_WITH_KNOTS('',3,(#12244,#12245,#12246,#12247,#12248,
#12249,#12250,#12251,#12252,#12253,#12254),.UNSPECIFIED.,.F.,.F.,(4,1,1,
1,1,1,1,1,4),(15.7079632679489,15.8530040996568,16.8508601235068,17.8487161473568,
18.8465721712069,19.8444281950569,20.8422842189069,21.8401402427569,21.9911485751285),
 .UNSPECIFIED.);
#344=B_SPLINE_CURVE_WITH_KNOTS('',3,(#12255,#12256,#12257,#12258,#12259,
#12260,#12261,#12262,#12263,#12264),.UNSPECIFIED.,.F.,.F.,(4,1,1,1,1,1,
1,4),(15.7079632679489,16.393853060477,17.391709084327,18.389565108177,
19.3874211320271,20.3852771558771,21.3831331797271,21.9911485751285),
 .UNSPECIFIED.);
#345=B_SPLINE_CURVE_WITH_KNOTS('',3,(#12429,#12430,#12431,#12432,#12433,
#12434,#12435,#12436,#12437,#12438,#12439,#12440,#12441,#12442,#12443,#12444,
#12445,#12446,#12447,#12448,#12449,#12450,#12451,#12452,#12453,#12454,#12455,
#12456,#12457,#12458,#12459,#12460,#12461,#12462,#12463,#12464,#12465,#12466,
#12467,#12468,#12469,#12470,#12471,#12472,#12473,#12474,#12475,#12476,#12477,
#12478,#12479,#12480),.UNSPECIFIED.,.F.,.F.,(4,3,3,3,3,3,3,3,3,3,3,3,3,
3,3,3,3,4),(0.,0.0396840521468864,0.059875020004076,0.0739768413530052,
0.0859734763696041,0.12472674289153,0.15053968360953,0.161721130091714,
0.197217246712606,0.224559338868372,0.235244538191998,0.270292231220177,
0.290140832661352,0.305406213186563,0.333032234601024,0.347218928912509,
0.375435310304714,0.378621596831395),.UNSPECIFIED.);
#346=B_SPLINE_CURVE_WITH_KNOTS('',3,(#12481,#12482,#12483,#12484,#12485,
#12486,#12487,#12488,#12489,#12490,#12491,#12492,#12493,#12494,#12495,#12496,
#12497,#12498,#12499,#12500,#12501,#12502,#12503,#12504,#12505,#12506,#12507,
#12508,#12509,#12510,#12511,#12512,#12513,#12514,#12515,#12516,#12517,#12518,
#12519,#12520,#12521,#12522,#12523,#12524,#12525,#12526,#12527,#12528,#12529,
#12530,#12531,#12532),.UNSPECIFIED.,.F.,.F.,(4,3,3,3,3,3,3,3,3,3,3,3,3,
3,3,3,3,4),(0.,0.0336993562019562,0.0587206748846584,0.0734845893515782,
0.10979434417143,0.132864732420192,0.14363295898452,0.177258566323581,0.196035872055507,
0.207661896409673,0.24493922230234,0.26977275930509,0.282653420233469,0.310317023711199,
0.326845507637221,0.342480201732081,0.373057649428629,0.376940817211641),
 .UNSPECIFIED.);
#347=B_SPLINE_CURVE_WITH_KNOTS('',3,(#12533,#12534,#12535,#12536,#12537,
#12538,#12539,#12540,#12541,#12542,#12543,#12544,#12545,#12546,#12547,#12548,
#12549,#12550,#12551,#12552,#12553,#12554,#12555,#12556,#12557),
 .UNSPECIFIED.,.F.,.F.,(4,3,3,3,3,3,3,3,4),(-10.1295685708718,-9.97856023850017,
-8.98070421465016,-7.98284819080014,-6.98499216695012,-5.9871361431001,
-4.98928011925009,-3.99142409540007,-3.84638326369223),.UNSPECIFIED.);
#348=B_SPLINE_CURVE_WITH_KNOTS('',3,(#12722,#12723,#12724,#12725,#12726,
#12727,#12728,#12729,#12730,#12731,#12732,#12733,#12734,#12735,#12736,#12737,
#12738,#12739,#12740,#12741,#12742,#12743,#12744,#12745,#12746,#12747,#12748,
#12749,#12750,#12751,#12752,#12753,#12754,#12755,#12756,#12757,#12758,#12759,
#12760,#12761,#12762,#12763,#12764,#12765,#12766,#12767,#12768,#12769,#12770,
#12771,#12772,#12773),.UNSPECIFIED.,.F.,.F.,(4,3,3,3,3,3,3,3,3,3,3,3,3,
3,3,3,3,4),(0.,0.0336994181656691,0.058720699944575,0.0734845927808491,
0.109794365269302,0.132864771817205,0.143633027430854,0.177258566323583,
0.196035861323974,0.207661888854805,0.244939171913457,0.269772630388177,
0.282653282483456,0.310316825068278,0.326842481101116,0.3424799795213,0.373057649428634,
0.376940817211644),.UNSPECIFIED.);
#349=B_SPLINE_CURVE_WITH_KNOTS('',3,(#12774,#12775,#12776,#12777,#12778,
#12779,#12780,#12781,#12782,#12783,#12784,#12785,#12786,#12787,#12788,#12789,
#12790,#12791,#12792,#12793,#12794,#12795),.UNSPECIFIED.,.F.,.F.,(4,3,3,
3,3,3,3,4),(7.59300756235157,7.98284819080014,8.98070421465015,9.97856023850017,
10.9764162623502,11.9742722862002,12.9721283100502,13.8761928695312),
 .UNSPECIFIED.);
#350=B_SPLINE_CURVE_WITH_KNOTS('',3,(#12796,#12797,#12798,#12799,#12800,
#12801,#12802,#12803,#12804,#12805,#12806,#12807,#12808,#12809,#12810,#12811,
#12812,#12813,#12814,#12815,#12816,#12817,#12818,#12819,#12820,#12821,#12822,
#12823,#12824,#12825,#12826,#12827,#12828,#12829,#12830,#12831,#12832,#12833,
#12834,#12835,#12836,#12837,#12838,#12839,#12840,#12841,#12842,#12843,#12844,
#12845,#12846,#12847),.UNSPECIFIED.,.F.,.F.,(4,3,3,3,3,3,3,3,3,3,3,3,3,
3,3,3,3,4),(0.,0.0396840879963326,0.0598753046358157,0.0739780373014043,
0.0859735519163639,0.124726799518446,0.150539713843663,0.16172115065774,
0.19721724671262,0.224559319464973,0.235244508043305,0.270292208608664,
0.290140708581571,0.305406176565746,0.333032103859708,0.347218909613468,
0.37543531030474,0.378621596831421),.UNSPECIFIED.);
#351=SHAPE_REPRESENTATION_RELATIONSHIP('SRR','None',#13035,#363);
#352=SHAPE_REPRESENTATION_RELATIONSHIP('SRR','None',#13036,#364);
#353=SHAPE_REPRESENTATION_RELATIONSHIP('SRR','None',#13037,#365);
#354=SHAPE_REPRESENTATION_RELATIONSHIP('SRR','None',#13038,#366);
#355=SHAPE_REPRESENTATION_RELATIONSHIP('SRR','None',#13039,#367);
#356=SHAPE_REPRESENTATION_RELATIONSHIP('SRR','None',#13040,#368);
#357=SHAPE_REPRESENTATION_RELATIONSHIP('SRR','None',#13041,#369);
#358=SHAPE_REPRESENTATION_RELATIONSHIP('SRR','None',#13042,#370);
#359=SHAPE_REPRESENTATION_RELATIONSHIP('SRR','None',#13043,#371);
#360=SHAPE_REPRESENTATION_RELATIONSHIP('SRR','None',#13044,#372);
#361=SHAPE_REPRESENTATION_RELATIONSHIP('SRR','None',#13045,#373);
#362=SHAPE_REPRESENTATION_RELATIONSHIP('SRR','None',#13046,#374);
#363=ADVANCED_BREP_SHAPE_REPRESENTATION('',(#387),#12951);
#364=ADVANCED_BREP_SHAPE_REPRESENTATION('',(#388),#12952);
#365=ADVANCED_BREP_SHAPE_REPRESENTATION('',(#389),#12953);
#366=ADVANCED_BREP_SHAPE_REPRESENTATION('',(#390),#12954);
#367=ADVANCED_BREP_SHAPE_REPRESENTATION('',(#391),#12955);
#368=ADVANCED_BREP_SHAPE_REPRESENTATION('',(#392),#12956);
#369=ADVANCED_BREP_SHAPE_REPRESENTATION('',(#393),#12957);
#370=ADVANCED_BREP_SHAPE_REPRESENTATION('',(#394),#12958);
#371=ADVANCED_BREP_SHAPE_REPRESENTATION('',(#395),#12959);
#372=ADVANCED_BREP_SHAPE_REPRESENTATION('',(#396),#12960);
#373=ADVANCED_BREP_SHAPE_REPRESENTATION('',(#397),#12961);
#374=ADVANCED_BREP_SHAPE_REPRESENTATION('',(#398),#12962);
#375=STYLED_ITEM('',(#13104),#387);
#376=STYLED_ITEM('',(#13105),#388);
#377=STYLED_ITEM('',(#13106),#389);
#378=STYLED_ITEM('',(#13107),#390);
#379=STYLED_ITEM('',(#13108),#391);
#380=STYLED_ITEM('',(#13109),#392);
#381=STYLED_ITEM('',(#13110),#393);
#382=STYLED_ITEM('',(#13111),#394);
#383=STYLED_ITEM('',(#13112),#395);
#384=STYLED_ITEM('',(#13113),#396);
#385=STYLED_ITEM('',(#13114),#397);
#386=STYLED_ITEM('',(#13115),#398);
#387=MANIFOLD_SOLID_BREP('Body1',#4809);
#388=MANIFOLD_SOLID_BREP('Body1',#4810);
#389=MANIFOLD_SOLID_BREP('Body1',#4811);
#390=MANIFOLD_SOLID_BREP('Body1',#4812);
#391=MANIFOLD_SOLID_BREP('Body1',#4813);
#392=MANIFOLD_SOLID_BREP('Body1',#4814);
#393=MANIFOLD_SOLID_BREP('Body1',#4815);
#394=MANIFOLD_SOLID_BREP('Body1',#4816);
#395=MANIFOLD_SOLID_BREP('Body1',#4817);
#396=MANIFOLD_SOLID_BREP('Body1',#4818);
#397=MANIFOLD_SOLID_BREP('Body1',#4819);
#398=MANIFOLD_SOLID_BREP('Body1',#4820);
#399=FACE_BOUND('',#830,.T.);
#400=FACE_BOUND('',#833,.T.);
#401=FACE_BOUND('',#852,.T.);
#402=FACE_BOUND('',#859,.T.);
#403=FACE_BOUND('',#867,.T.);
#404=FACE_BOUND('',#868,.T.);
#405=FACE_BOUND('',#869,.T.);
#406=FACE_BOUND('',#870,.T.);
#407=FACE_BOUND('',#871,.T.);
#408=FACE_BOUND('',#872,.T.);
#409=FACE_BOUND('',#892,.T.);
#410=FACE_BOUND('',#899,.T.);
#411=FACE_BOUND('',#907,.T.);
#412=FACE_BOUND('',#908,.T.);
#413=FACE_BOUND('',#909,.T.);
#414=FACE_BOUND('',#910,.T.);
#415=FACE_BOUND('',#911,.T.);
#416=FACE_BOUND('',#912,.T.);
#417=FACE_BOUND('',#945,.T.);
#418=FACE_BOUND('',#946,.T.);
#419=FACE_BOUND('',#947,.T.);
#420=FACE_BOUND('',#950,.T.);
#421=FACE_BOUND('',#951,.T.);
#422=FACE_BOUND('',#952,.T.);
#423=FACE_BOUND('',#962,.T.);
#424=FACE_BOUND('',#963,.T.);
#425=FACE_BOUND('',#970,.T.);
#426=FACE_BOUND('',#972,.T.);
#427=FACE_BOUND('',#973,.T.);
#428=FACE_BOUND('',#979,.T.);
#429=FACE_BOUND('',#985,.T.);
#430=FACE_BOUND('',#986,.T.);
#431=FACE_BOUND('',#992,.T.);
#432=FACE_BOUND('',#996,.T.);
#433=FACE_BOUND('',#998,.T.);
#434=FACE_BOUND('',#999,.T.);
#435=FACE_BOUND('',#1003,.T.);
#436=FACE_BOUND('',#1006,.T.);
#437=FACE_BOUND('',#1092,.T.);
#438=FACE_BOUND('',#1095,.T.);
#439=FACE_BOUND('',#1113,.T.);
#440=FACE_BOUND('',#1122,.T.);
#441=PLANE('',#4959);
#442=PLANE('',#4964);
#443=PLANE('',#4969);
#444=PLANE('',#4973);
#445=PLANE('',#4977);
#446=PLANE('',#4981);
#447=PLANE('',#4986);
#448=PLANE('',#4987);
#449=PLANE('',#4988);
#450=PLANE('',#4989);
#451=PLANE('',#4990);
#452=PLANE('',#4991);
#453=PLANE('',#4992);
#454=PLANE('',#4993);
#455=PLANE('',#4994);
#456=PLANE('',#4995);
#457=PLANE('',#4996);
#458=PLANE('',#4997);
#459=PLANE('',#4998);
#460=PLANE('',#4999);
#461=PLANE('',#5000);
#462=PLANE('',#5001);
#463=PLANE('',#5002);
#464=PLANE('',#5003);
#465=PLANE('',#5004);
#466=PLANE('',#5005);
#467=PLANE('',#5006);
#468=PLANE('',#5007);
#469=PLANE('',#5012);
#470=PLANE('',#5016);
#471=PLANE('',#5020);
#472=PLANE('',#5024);
#473=PLANE('',#5031);
#474=PLANE('',#5032);
#475=PLANE('',#5033);
#476=PLANE('',#5034);
#477=PLANE('',#5035);
#478=PLANE('',#5036);
#479=PLANE('',#5037);
#480=PLANE('',#5038);
#481=PLANE('',#5039);
#482=PLANE('',#5040);
#483=PLANE('',#5041);
#484=PLANE('',#5042);
#485=PLANE('',#5043);
#486=PLANE('',#5044);
#487=PLANE('',#5045);
#488=PLANE('',#5046);
#489=PLANE('',#5047);
#490=PLANE('',#5048);
#491=PLANE('',#5049);
#492=PLANE('',#5050);
#493=PLANE('',#5051);
#494=PLANE('',#5052);
#495=PLANE('',#5054);
#496=PLANE('',#5055);
#497=PLANE('',#5056);
#498=PLANE('',#5057);
#499=PLANE('',#5058);
#500=PLANE('',#5059);
#501=PLANE('',#5060);
#502=PLANE('',#5061);
#503=PLANE('',#5062);
#504=PLANE('',#5063);
#505=PLANE('',#5065);
#506=PLANE('',#5066);
#507=PLANE('',#5067);
#508=PLANE('',#5068);
#509=PLANE('',#5069);
#510=PLANE('',#5070);
#511=PLANE('',#5072);
#512=PLANE('',#5073);
#513=PLANE('',#5074);
#514=PLANE('',#5075);
#515=PLANE('',#5076);
#516=PLANE('',#5077);
#517=PLANE('',#5078);
#518=PLANE('',#5079);
#519=PLANE('',#5081);
#520=PLANE('',#5085);
#521=PLANE('',#5095);
#522=PLANE('',#5096);
#523=PLANE('',#5097);
#524=PLANE('',#5098);
#525=PLANE('',#5099);
#526=PLANE('',#5100);
#527=PLANE('',#5108);
#528=PLANE('',#5112);
#529=PLANE('',#5113);
#530=PLANE('',#5114);
#531=PLANE('',#5115);
#532=PLANE('',#5116);
#533=PLANE('',#5123);
#534=PLANE('',#5124);
#535=PLANE('',#5131);
#536=PLANE('',#5132);
#537=PLANE('',#5133);
#538=PLANE('',#5141);
#539=PLANE('',#5145);
#540=PLANE('',#5146);
#541=PLANE('',#5150);
#542=PLANE('',#5151);
#543=PLANE('',#5152);
#544=PLANE('',#5159);
#545=PLANE('',#5160);
#546=PLANE('',#5161);
#547=PLANE('',#5162);
#548=PLANE('',#5164);
#549=PLANE('',#5169);
#550=PLANE('',#5174);
#551=PLANE('',#5176);
#552=PLANE('',#5254);
#553=PLANE('',#5255);
#554=PLANE('',#5256);
#555=PLANE('',#5257);
#556=PLANE('',#5258);
#557=PLANE('',#5259);
#558=PLANE('',#5260);
#559=PLANE('',#5261);
#560=PLANE('',#5265);
#561=PLANE('',#5266);
#562=PLANE('',#5286);
#563=PLANE('',#5288);
#564=PLANE('',#5289);
#565=PLANE('',#5290);
#566=PLANE('',#5291);
#567=PLANE('',#5292);
#568=PLANE('',#5293);
#569=PLANE('',#5294);
#570=PLANE('',#5299);
#571=PLANE('',#5300);
#572=FACE_OUTER_BOUND('',#828,.T.);
#573=FACE_OUTER_BOUND('',#829,.T.);
#574=FACE_OUTER_BOUND('',#831,.T.);
#575=FACE_OUTER_BOUND('',#832,.T.);
#576=FACE_OUTER_BOUND('',#834,.T.);
#577=FACE_OUTER_BOUND('',#835,.T.);
#578=FACE_OUTER_BOUND('',#836,.T.);
#579=FACE_OUTER_BOUND('',#837,.T.);
#580=FACE_OUTER_BOUND('',#838,.T.);
#581=FACE_OUTER_BOUND('',#839,.T.);
#582=FACE_OUTER_BOUND('',#840,.T.);
#583=FACE_OUTER_BOUND('',#841,.T.);
#584=FACE_OUTER_BOUND('',#842,.T.);
#585=FACE_OUTER_BOUND('',#843,.T.);
#586=FACE_OUTER_BOUND('',#844,.T.);
#587=FACE_OUTER_BOUND('',#845,.T.);
#588=FACE_OUTER_BOUND('',#846,.T.);
#589=FACE_OUTER_BOUND('',#847,.T.);
#590=FACE_OUTER_BOUND('',#848,.T.);
#591=FACE_OUTER_BOUND('',#849,.T.);
#592=FACE_OUTER_BOUND('',#850,.T.);
#593=FACE_OUTER_BOUND('',#851,.T.);
#594=FACE_OUTER_BOUND('',#853,.T.);
#595=FACE_OUTER_BOUND('',#854,.T.);
#596=FACE_OUTER_BOUND('',#855,.T.);
#597=FACE_OUTER_BOUND('',#856,.T.);
#598=FACE_OUTER_BOUND('',#857,.T.);
#599=FACE_OUTER_BOUND('',#858,.T.);
#600=FACE_OUTER_BOUND('',#860,.T.);
#601=FACE_OUTER_BOUND('',#861,.T.);
#602=FACE_OUTER_BOUND('',#862,.T.);
#603=FACE_OUTER_BOUND('',#863,.T.);
#604=FACE_OUTER_BOUND('',#864,.T.);
#605=FACE_OUTER_BOUND('',#865,.T.);
#606=FACE_OUTER_BOUND('',#866,.T.);
#607=FACE_OUTER_BOUND('',#873,.T.);
#608=FACE_OUTER_BOUND('',#874,.T.);
#609=FACE_OUTER_BOUND('',#875,.T.);
#610=FACE_OUTER_BOUND('',#876,.T.);
#611=FACE_OUTER_BOUND('',#877,.T.);
#612=FACE_OUTER_BOUND('',#878,.T.);
#613=FACE_OUTER_BOUND('',#879,.T.);
#614=FACE_OUTER_BOUND('',#880,.T.);
#615=FACE_OUTER_BOUND('',#881,.T.);
#616=FACE_OUTER_BOUND('',#882,.T.);
#617=FACE_OUTER_BOUND('',#883,.T.);
#618=FACE_OUTER_BOUND('',#884,.T.);
#619=FACE_OUTER_BOUND('',#885,.T.);
#620=FACE_OUTER_BOUND('',#886,.T.);
#621=FACE_OUTER_BOUND('',#887,.T.);
#622=FACE_OUTER_BOUND('',#888,.T.);
#623=FACE_OUTER_BOUND('',#889,.T.);
#624=FACE_OUTER_BOUND('',#890,.T.);
#625=FACE_OUTER_BOUND('',#891,.T.);
#626=FACE_OUTER_BOUND('',#893,.T.);
#627=FACE_OUTER_BOUND('',#894,.T.);
#628=FACE_OUTER_BOUND('',#895,.T.);
#629=FACE_OUTER_BOUND('',#896,.T.);
#630=FACE_OUTER_BOUND('',#897,.T.);
#631=FACE_OUTER_BOUND('',#898,.T.);
#632=FACE_OUTER_BOUND('',#900,.T.);
#633=FACE_OUTER_BOUND('',#901,.T.);
#634=FACE_OUTER_BOUND('',#902,.T.);
#635=FACE_OUTER_BOUND('',#903,.T.);
#636=FACE_OUTER_BOUND('',#904,.T.);
#637=FACE_OUTER_BOUND('',#905,.T.);
#638=FACE_OUTER_BOUND('',#906,.T.);
#639=FACE_OUTER_BOUND('',#913,.T.);
#640=FACE_OUTER_BOUND('',#914,.T.);
#641=FACE_OUTER_BOUND('',#915,.T.);
#642=FACE_OUTER_BOUND('',#916,.T.);
#643=FACE_OUTER_BOUND('',#917,.T.);
#644=FACE_OUTER_BOUND('',#918,.T.);
#645=FACE_OUTER_BOUND('',#919,.T.);
#646=FACE_OUTER_BOUND('',#920,.T.);
#647=FACE_OUTER_BOUND('',#921,.T.);
#648=FACE_OUTER_BOUND('',#922,.T.);
#649=FACE_OUTER_BOUND('',#923,.T.);
#650=FACE_OUTER_BOUND('',#924,.T.);
#651=FACE_OUTER_BOUND('',#925,.T.);
#652=FACE_OUTER_BOUND('',#926,.T.);
#653=FACE_OUTER_BOUND('',#927,.T.);
#654=FACE_OUTER_BOUND('',#928,.T.);
#655=FACE_OUTER_BOUND('',#929,.T.);
#656=FACE_OUTER_BOUND('',#930,.T.);
#657=FACE_OUTER_BOUND('',#931,.T.);
#658=FACE_OUTER_BOUND('',#932,.T.);
#659=FACE_OUTER_BOUND('',#933,.T.);
#660=FACE_OUTER_BOUND('',#934,.T.);
#661=FACE_OUTER_BOUND('',#935,.T.);
#662=FACE_OUTER_BOUND('',#936,.T.);
#663=FACE_OUTER_BOUND('',#937,.T.);
#664=FACE_OUTER_BOUND('',#938,.T.);
#665=FACE_OUTER_BOUND('',#939,.T.);
#666=FACE_OUTER_BOUND('',#940,.T.);
#667=FACE_OUTER_BOUND('',#941,.T.);
#668=FACE_OUTER_BOUND('',#942,.T.);
#669=FACE_OUTER_BOUND('',#943,.T.);
#670=FACE_OUTER_BOUND('',#944,.T.);
#671=FACE_OUTER_BOUND('',#948,.T.);
#672=FACE_OUTER_BOUND('',#949,.T.);
#673=FACE_OUTER_BOUND('',#953,.T.);
#674=FACE_OUTER_BOUND('',#954,.T.);
#675=FACE_OUTER_BOUND('',#955,.T.);
#676=FACE_OUTER_BOUND('',#956,.T.);
#677=FACE_OUTER_BOUND('',#957,.T.);
#678=FACE_OUTER_BOUND('',#958,.T.);
#679=FACE_OUTER_BOUND('',#959,.T.);
#680=FACE_OUTER_BOUND('',#960,.T.);
#681=FACE_OUTER_BOUND('',#961,.T.);
#682=FACE_OUTER_BOUND('',#964,.T.);
#683=FACE_OUTER_BOUND('',#965,.T.);
#684=FACE_OUTER_BOUND('',#966,.T.);
#685=FACE_OUTER_BOUND('',#967,.T.);
#686=FACE_OUTER_BOUND('',#968,.T.);
#687=FACE_OUTER_BOUND('',#969,.T.);
#688=FACE_OUTER_BOUND('',#971,.T.);
#689=FACE_OUTER_BOUND('',#974,.T.);
#690=FACE_OUTER_BOUND('',#975,.T.);
#691=FACE_OUTER_BOUND('',#976,.T.);
#692=FACE_OUTER_BOUND('',#977,.T.);
#693=FACE_OUTER_BOUND('',#978,.T.);
#694=FACE_OUTER_BOUND('',#980,.T.);
#695=FACE_OUTER_BOUND('',#981,.T.);
#696=FACE_OUTER_BOUND('',#982,.T.);
#697=FACE_OUTER_BOUND('',#983,.T.);
#698=FACE_OUTER_BOUND('',#984,.T.);
#699=FACE_OUTER_BOUND('',#987,.T.);
#700=FACE_OUTER_BOUND('',#988,.T.);
#701=FACE_OUTER_BOUND('',#989,.T.);
#702=FACE_OUTER_BOUND('',#990,.T.);
#703=FACE_OUTER_BOUND('',#991,.T.);
#704=FACE_OUTER_BOUND('',#993,.T.);
#705=FACE_OUTER_BOUND('',#994,.T.);
#706=FACE_OUTER_BOUND('',#995,.T.);
#707=FACE_OUTER_BOUND('',#997,.T.);
#708=FACE_OUTER_BOUND('',#1000,.T.);
#709=FACE_OUTER_BOUND('',#1001,.T.);
#710=FACE_OUTER_BOUND('',#1002,.T.);
#711=FACE_OUTER_BOUND('',#1004,.T.);
#712=FACE_OUTER_BOUND('',#1005,.T.);
#713=FACE_OUTER_BOUND('',#1007,.T.);
#714=FACE_OUTER_BOUND('',#1008,.T.);
#715=FACE_OUTER_BOUND('',#1009,.T.);
#716=FACE_OUTER_BOUND('',#1010,.T.);
#717=FACE_OUTER_BOUND('',#1011,.T.);
#718=FACE_OUTER_BOUND('',#1012,.T.);
#719=FACE_OUTER_BOUND('',#1013,.T.);
#720=FACE_OUTER_BOUND('',#1014,.T.);
#721=FACE_OUTER_BOUND('',#1015,.T.);
#722=FACE_OUTER_BOUND('',#1016,.T.);
#723=FACE_OUTER_BOUND('',#1017,.T.);
#724=FACE_OUTER_BOUND('',#1018,.T.);
#725=FACE_OUTER_BOUND('',#1019,.T.);
#726=FACE_OUTER_BOUND('',#1020,.T.);
#727=FACE_OUTER_BOUND('',#1021,.T.);
#728=FACE_OUTER_BOUND('',#1022,.T.);
#729=FACE_OUTER_BOUND('',#1023,.T.);
#730=FACE_OUTER_BOUND('',#1024,.T.);
#731=FACE_OUTER_BOUND('',#1025,.T.);
#732=FACE_OUTER_BOUND('',#1026,.T.);
#733=FACE_OUTER_BOUND('',#1027,.T.);
#734=FACE_OUTER_BOUND('',#1028,.T.);
#735=FACE_OUTER_BOUND('',#1029,.T.);
#736=FACE_OUTER_BOUND('',#1030,.T.);
#737=FACE_OUTER_BOUND('',#1031,.T.);
#738=FACE_OUTER_BOUND('',#1032,.T.);
#739=FACE_OUTER_BOUND('',#1033,.T.);
#740=FACE_OUTER_BOUND('',#1034,.T.);
#741=FACE_OUTER_BOUND('',#1035,.T.);
#742=FACE_OUTER_BOUND('',#1036,.T.);
#743=FACE_OUTER_BOUND('',#1037,.T.);
#744=FACE_OUTER_BOUND('',#1038,.T.);
#745=FACE_OUTER_BOUND('',#1039,.T.);
#746=FACE_OUTER_BOUND('',#1040,.T.);
#747=FACE_OUTER_BOUND('',#1041,.T.);
#748=FACE_OUTER_BOUND('',#1042,.T.);
#749=FACE_OUTER_BOUND('',#1043,.T.);
#750=FACE_OUTER_BOUND('',#1044,.T.);
#751=FACE_OUTER_BOUND('',#1045,.T.);
#752=FACE_OUTER_BOUND('',#1046,.T.);
#753=FACE_OUTER_BOUND('',#1047,.T.);
#754=FACE_OUTER_BOUND('',#1048,.T.);
#755=FACE_OUTER_BOUND('',#1049,.T.);
#756=FACE_OUTER_BOUND('',#1050,.T.);
#757=FACE_OUTER_BOUND('',#1051,.T.);
#758=FACE_OUTER_BOUND('',#1052,.T.);
#759=FACE_OUTER_BOUND('',#1053,.T.);
#760=FACE_OUTER_BOUND('',#1054,.T.);
#761=FACE_OUTER_BOUND('',#1055,.T.);
#762=FACE_OUTER_BOUND('',#1056,.T.);
#763=FACE_OUTER_BOUND('',#1057,.T.);
#764=FACE_OUTER_BOUND('',#1058,.T.);
#765=FACE_OUTER_BOUND('',#1059,.T.);
#766=FACE_OUTER_BOUND('',#1060,.T.);
#767=FACE_OUTER_BOUND('',#1061,.T.);
#768=FACE_OUTER_BOUND('',#1062,.T.);
#769=FACE_OUTER_BOUND('',#1063,.T.);
#770=FACE_OUTER_BOUND('',#1064,.T.);
#771=FACE_OUTER_BOUND('',#1065,.T.);
#772=FACE_OUTER_BOUND('',#1066,.T.);
#773=FACE_OUTER_BOUND('',#1067,.T.);
#774=FACE_OUTER_BOUND('',#1068,.T.);
#775=FACE_OUTER_BOUND('',#1069,.T.);
#776=FACE_OUTER_BOUND('',#1070,.T.);
#777=FACE_OUTER_BOUND('',#1071,.T.);
#778=FACE_OUTER_BOUND('',#1072,.T.);
#779=FACE_OUTER_BOUND('',#1073,.T.);
#780=FACE_OUTER_BOUND('',#1074,.T.);
#781=FACE_OUTER_BOUND('',#1075,.T.);
#782=FACE_OUTER_BOUND('',#1076,.T.);
#783=FACE_OUTER_BOUND('',#1077,.T.);
#784=FACE_OUTER_BOUND('',#1078,.T.);
#785=FACE_OUTER_BOUND('',#1079,.T.);
#786=FACE_OUTER_BOUND('',#1080,.T.);
#787=FACE_OUTER_BOUND('',#1081,.T.);
#788=FACE_OUTER_BOUND('',#1082,.T.);
#789=FACE_OUTER_BOUND('',#1083,.T.);
#790=FACE_OUTER_BOUND('',#1084,.T.);
#791=FACE_OUTER_BOUND('',#1085,.T.);
#792=FACE_OUTER_BOUND('',#1086,.T.);
#793=FACE_OUTER_BOUND('',#1087,.T.);
#794=FACE_OUTER_BOUND('',#1088,.T.);
#795=FACE_OUTER_BOUND('',#1089,.T.);
#796=FACE_OUTER_BOUND('',#1090,.T.);
#797=FACE_OUTER_BOUND('',#1091,.T.);
#798=FACE_OUTER_BOUND('',#1093,.T.);
#799=FACE_OUTER_BOUND('',#1094,.T.);
#800=FACE_OUTER_BOUND('',#1096,.T.);
#801=FACE_OUTER_BOUND('',#1097,.T.);
#802=FACE_OUTER_BOUND('',#1098,.T.);
#803=FACE_OUTER_BOUND('',#1099,.T.);
#804=FACE_OUTER_BOUND('',#1100,.T.);
#805=FACE_OUTER_BOUND('',#1101,.T.);
#806=FACE_OUTER_BOUND('',#1102,.T.);
#807=FACE_OUTER_BOUND('',#1103,.T.);
#808=FACE_OUTER_BOUND('',#1104,.T.);
#809=FACE_OUTER_BOUND('',#1105,.T.);
#810=FACE_OUTER_BOUND('',#1106,.T.);
#811=FACE_OUTER_BOUND('',#1107,.T.);
#812=FACE_OUTER_BOUND('',#1108,.T.);
#813=FACE_OUTER_BOUND('',#1109,.T.);
#814=FACE_OUTER_BOUND('',#1110,.T.);
#815=FACE_OUTER_BOUND('',#1111,.T.);
#816=FACE_OUTER_BOUND('',#1112,.T.);
#817=FACE_OUTER_BOUND('',#1114,.T.);
#818=FACE_OUTER_BOUND('',#1115,.T.);
#819=FACE_OUTER_BOUND('',#1116,.T.);
#820=FACE_OUTER_BOUND('',#1117,.T.);
#821=FACE_OUTER_BOUND('',#1118,.T.);
#822=FACE_OUTER_BOUND('',#1119,.T.);
#823=FACE_OUTER_BOUND('',#1120,.T.);
#824=FACE_OUTER_BOUND('',#1121,.T.);
#825=FACE_OUTER_BOUND('',#1123,.T.);
#826=FACE_OUTER_BOUND('',#1124,.T.);
#827=FACE_OUTER_BOUND('',#1125,.T.);
#828=EDGE_LOOP('',(#3112,#3113,#3114,#3115));
#829=EDGE_LOOP('',(#3116));
#830=EDGE_LOOP('',(#3117));
#831=EDGE_LOOP('',(#3118,#3119,#3120,#3121));
#832=EDGE_LOOP('',(#3122));
#833=EDGE_LOOP('',(#3123));
#834=EDGE_LOOP('',(#3124,#3125,#3126,#3127));
#835=EDGE_LOOP('',(#3128));
#836=EDGE_LOOP('',(#3129,#3130,#3131,#3132));
#837=EDGE_LOOP('',(#3133));
#838=EDGE_LOOP('',(#3134,#3135,#3136,#3137));
#839=EDGE_LOOP('',(#3138));
#840=EDGE_LOOP('',(#3139,#3140,#3141,#3142));
#841=EDGE_LOOP('',(#3143));
#842=EDGE_LOOP('',(#3144,#3145,#3146,#3147));
#843=EDGE_LOOP('',(#3148,#3149,#3150,#3151));
#844=EDGE_LOOP('',(#3152,#3153,#3154,#3155));
#845=EDGE_LOOP('',(#3156,#3157,#3158,#3159));
#846=EDGE_LOOP('',(#3160,#3161,#3162,#3163));
#847=EDGE_LOOP('',(#3164,#3165,#3166,#3167));
#848=EDGE_LOOP('',(#3168,#3169,#3170,#3171,#3172,#3173,#3174,#3175,#3176,
#3177,#3178,#3179,#3180,#3181,#3182,#3183,#3184,#3185,#3186,#3187));
#849=EDGE_LOOP('',(#3188,#3189,#3190,#3191));
#850=EDGE_LOOP('',(#3192,#3193,#3194,#3195));
#851=EDGE_LOOP('',(#3196,#3197,#3198,#3199));
#852=EDGE_LOOP('',(#3200));
#853=EDGE_LOOP('',(#3201,#3202,#3203,#3204));
#854=EDGE_LOOP('',(#3205,#3206,#3207,#3208));
#855=EDGE_LOOP('',(#3209,#3210,#3211,#3212));
#856=EDGE_LOOP('',(#3213,#3214,#3215,#3216));
#857=EDGE_LOOP('',(#3217,#3218,#3219,#3220));
#858=EDGE_LOOP('',(#3221,#3222,#3223,#3224));
#859=EDGE_LOOP('',(#3225));
#860=EDGE_LOOP('',(#3226,#3227,#3228,#3229));
#861=EDGE_LOOP('',(#3230,#3231,#3232,#3233));
#862=EDGE_LOOP('',(#3234,#3235,#3236,#3237));
#863=EDGE_LOOP('',(#3238,#3239,#3240,#3241,#3242,#3243,#3244,#3245,#3246,
#3247,#3248,#3249));
#864=EDGE_LOOP('',(#3250,#3251,#3252,#3253));
#865=EDGE_LOOP('',(#3254,#3255,#3256,#3257,#3258,#3259,#3260,#3261,#3262,
#3263,#3264,#3265));
#866=EDGE_LOOP('',(#3266,#3267,#3268,#3269));
#867=EDGE_LOOP('',(#3270));
#868=EDGE_LOOP('',(#3271));
#869=EDGE_LOOP('',(#3272));
#870=EDGE_LOOP('',(#3273));
#871=EDGE_LOOP('',(#3274));
#872=EDGE_LOOP('',(#3275));
#873=EDGE_LOOP('',(#3276,#3277,#3278,#3279));
#874=EDGE_LOOP('',(#3280,#3281,#3282,#3283));
#875=EDGE_LOOP('',(#3284));
#876=EDGE_LOOP('',(#3285,#3286,#3287,#3288));
#877=EDGE_LOOP('',(#3289));
#878=EDGE_LOOP('',(#3290,#3291,#3292,#3293));
#879=EDGE_LOOP('',(#3294));
#880=EDGE_LOOP('',(#3295,#3296,#3297,#3298));
#881=EDGE_LOOP('',(#3299));
#882=EDGE_LOOP('',(#3300,#3301,#3302,#3303));
#883=EDGE_LOOP('',(#3304,#3305,#3306,#3307));
#884=EDGE_LOOP('',(#3308,#3309,#3310,#3311));
#885=EDGE_LOOP('',(#3312,#3313,#3314,#3315));
#886=EDGE_LOOP('',(#3316,#3317,#3318,#3319));
#887=EDGE_LOOP('',(#3320,#3321,#3322,#3323));
#888=EDGE_LOOP('',(#3324,#3325,#3326,#3327,#3328,#3329,#3330,#3331,#3332,
#3333,#3334,#3335,#3336,#3337,#3338,#3339,#3340,#3341,#3342,#3343));
#889=EDGE_LOOP('',(#3344,#3345,#3346,#3347));
#890=EDGE_LOOP('',(#3348,#3349,#3350,#3351));
#891=EDGE_LOOP('',(#3352,#3353,#3354,#3355));
#892=EDGE_LOOP('',(#3356));
#893=EDGE_LOOP('',(#3357,#3358,#3359,#3360));
#894=EDGE_LOOP('',(#3361,#3362,#3363,#3364));
#895=EDGE_LOOP('',(#3365,#3366,#3367,#3368));
#896=EDGE_LOOP('',(#3369,#3370,#3371,#3372));
#897=EDGE_LOOP('',(#3373,#3374,#3375,#3376));
#898=EDGE_LOOP('',(#3377,#3378,#3379,#3380));
#899=EDGE_LOOP('',(#3381));
#900=EDGE_LOOP('',(#3382,#3383,#3384,#3385));
#901=EDGE_LOOP('',(#3386,#3387,#3388,#3389));
#902=EDGE_LOOP('',(#3390,#3391,#3392,#3393));
#903=EDGE_LOOP('',(#3394,#3395,#3396,#3397,#3398,#3399,#3400,#3401,#3402,
#3403,#3404,#3405));
#904=EDGE_LOOP('',(#3406,#3407,#3408,#3409));
#905=EDGE_LOOP('',(#3410,#3411,#3412,#3413,#3414,#3415,#3416,#3417,#3418,
#3419,#3420,#3421));
#906=EDGE_LOOP('',(#3422,#3423,#3424,#3425));
#907=EDGE_LOOP('',(#3426));
#908=EDGE_LOOP('',(#3427));
#909=EDGE_LOOP('',(#3428));
#910=EDGE_LOOP('',(#3429));
#911=EDGE_LOOP('',(#3430));
#912=EDGE_LOOP('',(#3431));
#913=EDGE_LOOP('',(#3432,#3433,#3434,#3435));
#914=EDGE_LOOP('',(#3436,#3437,#3438,#3439));
#915=EDGE_LOOP('',(#3440,#3441,#3442,#3443));
#916=EDGE_LOOP('',(#3444,#3445,#3446,#3447));
#917=EDGE_LOOP('',(#3448,#3449,#3450,#3451,#3452,#3453,#3454,#3455));
#918=EDGE_LOOP('',(#3456,#3457,#3458,#3459));
#919=EDGE_LOOP('',(#3460,#3461,#3462,#3463));
#920=EDGE_LOOP('',(#3464,#3465,#3466,#3467));
#921=EDGE_LOOP('',(#3468,#3469,#3470,#3471,#3472,#3473,#3474,#3475));
#922=EDGE_LOOP('',(#3476,#3477,#3478,#3479));
#923=EDGE_LOOP('',(#3480,#3481,#3482,#3483));
#924=EDGE_LOOP('',(#3484,#3485,#3486,#3487));
#925=EDGE_LOOP('',(#3488,#3489,#3490,#3491));
#926=EDGE_LOOP('',(#3492,#3493,#3494,#3495));
#927=EDGE_LOOP('',(#3496,#3497,#3498,#3499));
#928=EDGE_LOOP('',(#3500,#3501,#3502,#3503));
#929=EDGE_LOOP('',(#3504,#3505,#3506,#3507));
#930=EDGE_LOOP('',(#3508,#3509,#3510,#3511));
#931=EDGE_LOOP('',(#3512,#3513,#3514,#3515));
#932=EDGE_LOOP('',(#3516,#3517,#3518,#3519));
#933=EDGE_LOOP('',(#3520,#3521,#3522,#3523));
#934=EDGE_LOOP('',(#3524,#3525,#3526,#3527));
#935=EDGE_LOOP('',(#3528,#3529,#3530,#3531));
#936=EDGE_LOOP('',(#3532,#3533,#3534,#3535,#3536,#3537));
#937=EDGE_LOOP('',(#3538,#3539,#3540,#3541,#3542,#3543));
#938=EDGE_LOOP('',(#3544,#3545,#3546,#3547));
#939=EDGE_LOOP('',(#3548,#3549,#3550,#3551));
#940=EDGE_LOOP('',(#3552,#3553,#3554,#3555));
#941=EDGE_LOOP('',(#3556,#3557,#3558,#3559));
#942=EDGE_LOOP('',(#3560,#3561,#3562,#3563));
#943=EDGE_LOOP('',(#3564,#3565,#3566,#3567));
#944=EDGE_LOOP('',(#3568,#3569,#3570,#3571));
#945=EDGE_LOOP('',(#3572,#3573,#3574,#3575));
#946=EDGE_LOOP('',(#3576));
#947=EDGE_LOOP('',(#3577));
#948=EDGE_LOOP('',(#3578,#3579,#3580,#3581));
#949=EDGE_LOOP('',(#3582,#3583,#3584,#3585));
#950=EDGE_LOOP('',(#3586,#3587,#3588,#3589));
#951=EDGE_LOOP('',(#3590));
#952=EDGE_LOOP('',(#3591));
#953=EDGE_LOOP('',(#3592,#3593,#3594,#3595));
#954=EDGE_LOOP('',(#3596,#3597,#3598,#3599));
#955=EDGE_LOOP('',(#3600,#3601,#3602,#3603));
#956=EDGE_LOOP('',(#3604,#3605,#3606,#3607));
#957=EDGE_LOOP('',(#3608,#3609,#3610,#3611));
#958=EDGE_LOOP('',(#3612,#3613,#3614,#3615));
#959=EDGE_LOOP('',(#3616,#3617,#3618,#3619));
#960=EDGE_LOOP('',(#3620,#3621,#3622,#3623));
#961=EDGE_LOOP('',(#3624,#3625,#3626,#3627,#3628,#3629,#3630,#3631,#3632,
#3633,#3634,#3635));
#962=EDGE_LOOP('',(#3636));
#963=EDGE_LOOP('',(#3637));
#964=EDGE_LOOP('',(#3638,#3639,#3640,#3641,#3642,#3643));
#965=EDGE_LOOP('',(#3644,#3645,#3646,#3647,#3648,#3649));
#966=EDGE_LOOP('',(#3650,#3651,#3652,#3653,#3654));
#967=EDGE_LOOP('',(#3655,#3656,#3657,#3658));
#968=EDGE_LOOP('',(#3659,#3660,#3661,#3662));
#969=EDGE_LOOP('',(#3663,#3664,#3665,#3666));
#970=EDGE_LOOP('',(#3667,#3668,#3669));
#971=EDGE_LOOP('',(#3670,#3671,#3672,#3673,#3674,#3675,#3676,#3677,#3678,
#3679,#3680,#3681,#3682,#3683,#3684,#3685));
#972=EDGE_LOOP('',(#3686));
#973=EDGE_LOOP('',(#3687));
#974=EDGE_LOOP('',(#3688,#3689,#3690,#3691));
#975=EDGE_LOOP('',(#3692,#3693,#3694,#3695));
#976=EDGE_LOOP('',(#3696,#3697,#3698,#3699,#3700));
#977=EDGE_LOOP('',(#3701,#3702,#3703,#3704));
#978=EDGE_LOOP('',(#3705,#3706,#3707,#3708));
#979=EDGE_LOOP('',(#3709,#3710,#3711));
#980=EDGE_LOOP('',(#3712,#3713,#3714,#3715));
#981=EDGE_LOOP('',(#3716,#3717,#3718,#3719));
#982=EDGE_LOOP('',(#3720,#3721,#3722));
#983=EDGE_LOOP('',(#3723,#3724,#3725,#3726));
#984=EDGE_LOOP('',(#3727,#3728,#3729,#3730,#3731,#3732,#3733,#3734,#3735,
#3736,#3737,#3738));
#985=EDGE_LOOP('',(#3739));
#986=EDGE_LOOP('',(#3740));
#987=EDGE_LOOP('',(#3741,#3742,#3743,#3744,#3745,#3746,#3747,#3748,#3749,
#3750,#3751,#3752));
#988=EDGE_LOOP('',(#3753,#3754,#3755,#3756));
#989=EDGE_LOOP('',(#3757,#3758,#3759));
#990=EDGE_LOOP('',(#3760,#3761,#3762,#3763,#3764));
#991=EDGE_LOOP('',(#3765,#3766,#3767));
#992=EDGE_LOOP('',(#3768));
#993=EDGE_LOOP('',(#3769,#3770,#3771,#3772));
#994=EDGE_LOOP('',(#3773,#3774,#3775,#3776));
#995=EDGE_LOOP('',(#3777,#3778,#3779));
#996=EDGE_LOOP('',(#3780));
#997=EDGE_LOOP('',(#3781,#3782,#3783,#3784));
#998=EDGE_LOOP('',(#3785));
#999=EDGE_LOOP('',(#3786));
#1000=EDGE_LOOP('',(#3787,#3788,#3789,#3790));
#1001=EDGE_LOOP('',(#3791,#3792,#3793,#3794,#3795));
#1002=EDGE_LOOP('',(#3796));
#1003=EDGE_LOOP('',(#3797));
#1004=EDGE_LOOP('',(#3798,#3799,#3800,#3801));
#1005=EDGE_LOOP('',(#3802));
#1006=EDGE_LOOP('',(#3803));
#1007=EDGE_LOOP('',(#3804,#3805,#3806,#3807));
#1008=EDGE_LOOP('',(#3808));
#1009=EDGE_LOOP('',(#3809,#3810,#3811,#3812));
#1010=EDGE_LOOP('',(#3813));
#1011=EDGE_LOOP('',(#3814,#3815,#3816,#3817));
#1012=EDGE_LOOP('',(#3818,#3819,#3820,#3821));
#1013=EDGE_LOOP('',(#3822,#3823,#3824,#3825));
#1014=EDGE_LOOP('',(#3826,#3827,#3828,#3829));
#1015=EDGE_LOOP('',(#3830,#3831,#3832,#3833));
#1016=EDGE_LOOP('',(#3834,#3835,#3836,#3837));
#1017=EDGE_LOOP('',(#3838,#3839,#3840,#3841));
#1018=EDGE_LOOP('',(#3842,#3843,#3844,#3845));
#1019=EDGE_LOOP('',(#3846,#3847,#3848,#3849));
#1020=EDGE_LOOP('',(#3850,#3851,#3852,#3853));
#1021=EDGE_LOOP('',(#3854,#3855,#3856,#3857));
#1022=EDGE_LOOP('',(#3858,#3859,#3860,#3861));
#1023=EDGE_LOOP('',(#3862,#3863,#3864,#3865));
#1024=EDGE_LOOP('',(#3866,#3867,#3868,#3869));
#1025=EDGE_LOOP('',(#3870,#3871,#3872,#3873));
#1026=EDGE_LOOP('',(#3874,#3875,#3876,#3877));
#1027=EDGE_LOOP('',(#3878,#3879,#3880,#3881));
#1028=EDGE_LOOP('',(#3882,#3883,#3884,#3885));
#1029=EDGE_LOOP('',(#3886,#3887,#3888,#3889));
#1030=EDGE_LOOP('',(#3890,#3891,#3892,#3893));
#1031=EDGE_LOOP('',(#3894,#3895,#3896,#3897));
#1032=EDGE_LOOP('',(#3898,#3899,#3900,#3901));
#1033=EDGE_LOOP('',(#3902,#3903,#3904,#3905));
#1034=EDGE_LOOP('',(#3906,#3907,#3908,#3909));
#1035=EDGE_LOOP('',(#3910,#3911,#3912,#3913));
#1036=EDGE_LOOP('',(#3914,#3915,#3916,#3917));
#1037=EDGE_LOOP('',(#3918,#3919,#3920,#3921));
#1038=EDGE_LOOP('',(#3922,#3923,#3924,#3925));
#1039=EDGE_LOOP('',(#3926,#3927,#3928,#3929));
#1040=EDGE_LOOP('',(#3930,#3931,#3932,#3933));
#1041=EDGE_LOOP('',(#3934,#3935,#3936,#3937));
#1042=EDGE_LOOP('',(#3938,#3939,#3940,#3941));
#1043=EDGE_LOOP('',(#3942,#3943,#3944,#3945));
#1044=EDGE_LOOP('',(#3946,#3947,#3948,#3949));
#1045=EDGE_LOOP('',(#3950,#3951,#3952,#3953,#3954));
#1046=EDGE_LOOP('',(#3955,#3956,#3957,#3958));
#1047=EDGE_LOOP('',(#3959,#3960,#3961,#3962));
#1048=EDGE_LOOP('',(#3963,#3964,#3965,#3966));
#1049=EDGE_LOOP('',(#3967,#3968,#3969,#3970));
#1050=EDGE_LOOP('',(#3971,#3972,#3973,#3974));
#1051=EDGE_LOOP('',(#3975,#3976,#3977,#3978));
#1052=EDGE_LOOP('',(#3979,#3980,#3981,#3982));
#1053=EDGE_LOOP('',(#3983,#3984,#3985,#3986));
#1054=EDGE_LOOP('',(#3987,#3988,#3989,#3990));
#1055=EDGE_LOOP('',(#3991,#3992,#3993,#3994));
#1056=EDGE_LOOP('',(#3995,#3996,#3997,#3998));
#1057=EDGE_LOOP('',(#3999,#4000,#4001,#4002));
#1058=EDGE_LOOP('',(#4003,#4004,#4005,#4006));
#1059=EDGE_LOOP('',(#4007,#4008,#4009,#4010));
#1060=EDGE_LOOP('',(#4011,#4012,#4013,#4014));
#1061=EDGE_LOOP('',(#4015,#4016,#4017,#4018));
#1062=EDGE_LOOP('',(#4019,#4020,#4021,#4022));
#1063=EDGE_LOOP('',(#4023,#4024,#4025,#4026));
#1064=EDGE_LOOP('',(#4027,#4028,#4029,#4030));
#1065=EDGE_LOOP('',(#4031,#4032,#4033,#4034));
#1066=EDGE_LOOP('',(#4035,#4036,#4037,#4038));
#1067=EDGE_LOOP('',(#4039,#4040,#4041,#4042));
#1068=EDGE_LOOP('',(#4043,#4044,#4045,#4046));
#1069=EDGE_LOOP('',(#4047,#4048,#4049,#4050));
#1070=EDGE_LOOP('',(#4051,#4052,#4053,#4054));
#1071=EDGE_LOOP('',(#4055,#4056,#4057,#4058));
#1072=EDGE_LOOP('',(#4059,#4060,#4061,#4062));
#1073=EDGE_LOOP('',(#4063,#4064,#4065,#4066));
#1074=EDGE_LOOP('',(#4067,#4068,#4069,#4070));
#1075=EDGE_LOOP('',(#4071,#4072,#4073,#4074));
#1076=EDGE_LOOP('',(#4075,#4076,#4077,#4078));
#1077=EDGE_LOOP('',(#4079,#4080,#4081,#4082));
#1078=EDGE_LOOP('',(#4083,#4084,#4085,#4086));
#1079=EDGE_LOOP('',(#4087,#4088,#4089,#4090));
#1080=EDGE_LOOP('',(#4091,#4092,#4093,#4094,#4095,#4096,#4097,#4098,#4099,
#4100,#4101,#4102,#4103,#4104,#4105,#4106,#4107,#4108,#4109,#4110,#4111,
#4112,#4113,#4114,#4115,#4116,#4117,#4118,#4119,#4120,#4121,#4122,#4123,
#4124,#4125,#4126,#4127,#4128,#4129,#4130,#4131,#4132,#4133,#4134,#4135,
#4136,#4137,#4138,#4139,#4140,#4141,#4142,#4143,#4144,#4145,#4146,#4147,
#4148,#4149,#4150,#4151,#4152,#4153,#4154,#4155,#4156,#4157,#4158,#4159,
#4160,#4161,#4162,#4163));
#1081=EDGE_LOOP('',(#4164,#4165,#4166,#4167));
#1082=EDGE_LOOP('',(#4168,#4169,#4170,#4171,#4172,#4173,#4174,#4175,#4176,
#4177,#4178,#4179,#4180,#4181,#4182,#4183,#4184,#4185,#4186,#4187,#4188,
#4189,#4190,#4191,#4192,#4193,#4194,#4195,#4196,#4197,#4198,#4199,#4200,
#4201,#4202,#4203,#4204,#4205,#4206,#4207,#4208,#4209,#4210,#4211,#4212,
#4213,#4214,#4215,#4216,#4217,#4218,#4219,#4220,#4221,#4222,#4223,#4224,
#4225,#4226,#4227,#4228,#4229,#4230,#4231,#4232,#4233,#4234,#4235,#4236,
#4237,#4238,#4239));
#1083=EDGE_LOOP('',(#4240,#4241,#4242));
#1084=EDGE_LOOP('',(#4243,#4244,#4245,#4246));
#1085=EDGE_LOOP('',(#4247,#4248,#4249,#4250));
#1086=EDGE_LOOP('',(#4251,#4252,#4253,#4254));
#1087=EDGE_LOOP('',(#4255,#4256,#4257,#4258));
#1088=EDGE_LOOP('',(#4259,#4260,#4261,#4262));
#1089=EDGE_LOOP('',(#4263,#4264,#4265,#4266));
#1090=EDGE_LOOP('',(#4267,#4268,#4269,#4270,#4271,#4272));
#1091=EDGE_LOOP('',(#4273));
#1092=EDGE_LOOP('',(#4274,#4275,#4276,#4277));
#1093=EDGE_LOOP('',(#4278,#4279,#4280,#4281));
#1094=EDGE_LOOP('',(#4282));
#1095=EDGE_LOOP('',(#4283,#4284,#4285,#4286,#4287,#4288));
#1096=EDGE_LOOP('',(#4289,#4290,#4291,#4292,#4293));
#1097=EDGE_LOOP('',(#4294,#4295,#4296));
#1098=EDGE_LOOP('',(#4297,#4298,#4299,#4300,#4301));
#1099=EDGE_LOOP('',(#4302,#4303,#4304,#4305));
#1100=EDGE_LOOP('',(#4306,#4307,#4308,#4309));
#1101=EDGE_LOOP('',(#4310,#4311,#4312,#4313));
#1102=EDGE_LOOP('',(#4314,#4315,#4316,#4317));
#1103=EDGE_LOOP('',(#4318,#4319,#4320,#4321));
#1104=EDGE_LOOP('',(#4322,#4323,#4324,#4325));
#1105=EDGE_LOOP('',(#4326,#4327,#4328,#4329));
#1106=EDGE_LOOP('',(#4330,#4331,#4332,#4333));
#1107=EDGE_LOOP('',(#4334,#4335,#4336,#4337));
#1108=EDGE_LOOP('',(#4338,#4339,#4340,#4341));
#1109=EDGE_LOOP('',(#4342,#4343,#4344,#4345));
#1110=EDGE_LOOP('',(#4346,#4347,#4348,#4349,#4350,#4351,#4352,#4353,#4354,
#4355,#4356,#4357,#4358,#4359,#4360,#4361));
#1111=EDGE_LOOP('',(#4362,#4363,#4364,#4365,#4366,#4367,#4368,#4369,#4370,
#4371,#4372,#4373,#4374,#4375,#4376));
#1112=EDGE_LOOP('',(#4377,#4378,#4379,#4380,#4381,#4382));
#1113=EDGE_LOOP('',(#4383,#4384,#4385,#4386));
#1114=EDGE_LOOP('',(#4387,#4388,#4389,#4390));
#1115=EDGE_LOOP('',(#4391,#4392,#4393,#4394));
#1116=EDGE_LOOP('',(#4395,#4396,#4397,#4398));
#1117=EDGE_LOOP('',(#4399,#4400,#4401,#4402));
#1118=EDGE_LOOP('',(#4403,#4404,#4405,#4406));
#1119=EDGE_LOOP('',(#4407,#4408,#4409,#4410));
#1120=EDGE_LOOP('',(#4411,#4412,#4413,#4414));
#1121=EDGE_LOOP('',(#4415,#4416,#4417,#4418,#4419,#4420));
#1122=EDGE_LOOP('',(#4421,#4422,#4423,#4424,#4425));
#1123=EDGE_LOOP('',(#4426,#4427,#4428,#4429));
#1124=EDGE_LOOP('',(#4430));
#1125=EDGE_LOOP('',(#4431));
#1126=LINE('',#6523,#1528);
#1127=LINE('',#6532,#1529);
#1128=LINE('',#6541,#1530);
#1129=LINE('',#6548,#1531);
#1130=LINE('',#6555,#1532);
#1131=LINE('',#6562,#1533);
#1132=LINE('',#6568,#1534);
#1133=LINE('',#6572,#1535);
#1134=LINE('',#6576,#1536);
#1135=LINE('',#6578,#1537);
#1136=LINE('',#6580,#1538);
#1137=LINE('',#6581,#1539);
#1138=LINE('',#6585,#1540);
#1139=LINE('',#6587,#1541);
#1140=LINE('',#6589,#1542);
#1141=LINE('',#6590,#1543);
#1142=LINE('',#6594,#1544);
#1143=LINE('',#6596,#1545);
#1144=LINE('',#6598,#1546);
#1145=LINE('',#6599,#1547);
#1146=LINE('',#6603,#1548);
#1147=LINE('',#6605,#1549);
#1148=LINE('',#6607,#1550);
#1149=LINE('',#6608,#1551);
#1150=LINE('',#6611,#1552);
#1151=LINE('',#6613,#1553);
#1152=LINE('',#6615,#1554);
#1153=LINE('',#6617,#1555);
#1154=LINE('',#6618,#1556);
#1155=LINE('',#6620,#1557);
#1156=LINE('',#6622,#1558);
#1157=LINE('',#6623,#1559);
#1158=LINE('',#6625,#1560);
#1159=LINE('',#6627,#1561);
#1160=LINE('',#6629,#1562);
#1161=LINE('',#6631,#1563);
#1162=LINE('',#6632,#1564);
#1163=LINE('',#6634,#1565);
#1164=LINE('',#6636,#1566);
#1165=LINE('',#6637,#1567);
#1166=LINE('',#6640,#1568);
#1167=LINE('',#6641,#1569);
#1168=LINE('',#6644,#1570);
#1169=LINE('',#6645,#1571);
#1170=LINE('',#6648,#1572);
#1171=LINE('',#6649,#1573);
#1172=LINE('',#6652,#1574);
#1173=LINE('',#6653,#1575);
#1174=LINE('',#6655,#1576);
#1175=LINE('',#6657,#1577);
#1176=LINE('',#6660,#1578);
#1177=LINE('',#6661,#1579);
#1178=LINE('',#6664,#1580);
#1179=LINE('',#6665,#1581);
#1180=LINE('',#6668,#1582);
#1181=LINE('',#6669,#1583);
#1182=LINE('',#6672,#1584);
#1183=LINE('',#6673,#1585);
#1184=LINE('',#6675,#1586);
#1185=LINE('',#6677,#1587);
#1186=LINE('',#6680,#1588);
#1187=LINE('',#6682,#1589);
#1188=LINE('',#6683,#1590);
#1189=LINE('',#6686,#1591);
#1190=LINE('',#6687,#1592);
#1191=LINE('',#6690,#1593);
#1192=LINE('',#6691,#1594);
#1193=LINE('',#6693,#1595);
#1194=LINE('',#6700,#1596);
#1195=LINE('',#6707,#1597);
#1196=LINE('',#6714,#1598);
#1197=LINE('',#6721,#1599);
#1198=LINE('',#6728,#1600);
#1199=LINE('',#6734,#1601);
#1200=LINE('',#6739,#1602);
#1201=LINE('',#6741,#1603);
#1202=LINE('',#6743,#1604);
#1203=LINE('',#6744,#1605);
#1204=LINE('',#6748,#1606);
#1205=LINE('',#6750,#1607);
#1206=LINE('',#6752,#1608);
#1207=LINE('',#6753,#1609);
#1208=LINE('',#6757,#1610);
#1209=LINE('',#6759,#1611);
#1210=LINE('',#6761,#1612);
#1211=LINE('',#6762,#1613);
#1212=LINE('',#6766,#1614);
#1213=LINE('',#6768,#1615);
#1214=LINE('',#6770,#1616);
#1215=LINE('',#6771,#1617);
#1216=LINE('',#6774,#1618);
#1217=LINE('',#6776,#1619);
#1218=LINE('',#6778,#1620);
#1219=LINE('',#6780,#1621);
#1220=LINE('',#6781,#1622);
#1221=LINE('',#6783,#1623);
#1222=LINE('',#6785,#1624);
#1223=LINE('',#6786,#1625);
#1224=LINE('',#6788,#1626);
#1225=LINE('',#6790,#1627);
#1226=LINE('',#6792,#1628);
#1227=LINE('',#6794,#1629);
#1228=LINE('',#6795,#1630);
#1229=LINE('',#6797,#1631);
#1230=LINE('',#6799,#1632);
#1231=LINE('',#6800,#1633);
#1232=LINE('',#6803,#1634);
#1233=LINE('',#6804,#1635);
#1234=LINE('',#6807,#1636);
#1235=LINE('',#6808,#1637);
#1236=LINE('',#6811,#1638);
#1237=LINE('',#6812,#1639);
#1238=LINE('',#6815,#1640);
#1239=LINE('',#6816,#1641);
#1240=LINE('',#6818,#1642);
#1241=LINE('',#6820,#1643);
#1242=LINE('',#6823,#1644);
#1243=LINE('',#6824,#1645);
#1244=LINE('',#6827,#1646);
#1245=LINE('',#6828,#1647);
#1246=LINE('',#6831,#1648);
#1247=LINE('',#6832,#1649);
#1248=LINE('',#6835,#1650);
#1249=LINE('',#6836,#1651);
#1250=LINE('',#6838,#1652);
#1251=LINE('',#6840,#1653);
#1252=LINE('',#6843,#1654);
#1253=LINE('',#6845,#1655);
#1254=LINE('',#6846,#1656);
#1255=LINE('',#6849,#1657);
#1256=LINE('',#6850,#1658);
#1257=LINE('',#6853,#1659);
#1258=LINE('',#6854,#1660);
#1259=LINE('',#6856,#1661);
#1260=LINE('',#6862,#1662);
#1261=LINE('',#6864,#1663);
#1262=LINE('',#6866,#1664);
#1263=LINE('',#6867,#1665);
#1264=LINE('',#6871,#1666);
#1265=LINE('',#6873,#1667);
#1266=LINE('',#6875,#1668);
#1267=LINE('',#6876,#1669);
#1268=LINE('',#6878,#1670);
#1269=LINE('',#6879,#1671);
#1270=LINE('',#6882,#1672);
#1271=LINE('',#6884,#1673);
#1272=LINE('',#6886,#1674);
#1273=LINE('',#6888,#1675);
#1274=LINE('',#6889,#1676);
#1275=LINE('',#6892,#1677);
#1276=LINE('',#6893,#1678);
#1277=LINE('',#6896,#1679);
#1278=LINE('',#6898,#1680);
#1279=LINE('',#6899,#1681);
#1280=LINE('',#6902,#1682);
#1281=LINE('',#6903,#1683);
#1282=LINE('',#6905,#1684);
#1283=LINE('',#6906,#1685);
#1284=LINE('',#6913,#1686);
#1285=LINE('',#6915,#1687);
#1286=LINE('',#6917,#1688);
#1287=LINE('',#6918,#1689);
#1288=LINE('',#6921,#1690);
#1289=LINE('',#6923,#1691);
#1290=LINE('',#6924,#1692);
#1291=LINE('',#6927,#1693);
#1292=LINE('',#6929,#1694);
#1293=LINE('',#6930,#1695);
#1294=LINE('',#6932,#1696);
#1295=LINE('',#6933,#1697);
#1296=LINE('',#6940,#1698);
#1297=LINE('',#6942,#1699);
#1298=LINE('',#6944,#1700);
#1299=LINE('',#6945,#1701);
#1300=LINE('',#6948,#1702);
#1301=LINE('',#6950,#1703);
#1302=LINE('',#6951,#1704);
#1303=LINE('',#6954,#1705);
#1304=LINE('',#6956,#1706);
#1305=LINE('',#6957,#1707);
#1306=LINE('',#6960,#1708);
#1307=LINE('',#6962,#1709);
#1308=LINE('',#6963,#1710);
#1309=LINE('',#6966,#1711);
#1310=LINE('',#6968,#1712);
#1311=LINE('',#6969,#1713);
#1312=LINE('',#6971,#1714);
#1313=LINE('',#6972,#1715);
#1314=LINE('',#6979,#1716);
#1315=LINE('',#6981,#1717);
#1316=LINE('',#6983,#1718);
#1317=LINE('',#6984,#1719);
#1318=LINE('',#6989,#1720);
#1319=LINE('',#6993,#1721);
#1320=LINE('',#6995,#1722);
#1321=LINE('',#6996,#1723);
#1322=LINE('',#7004,#1724);
#1323=LINE('',#7010,#1725);
#1324=LINE('',#7015,#1726);
#1325=LINE('',#7017,#1727);
#1326=LINE('',#7019,#1728);
#1327=LINE('',#7020,#1729);
#1328=LINE('',#7023,#1730);
#1329=LINE('',#7025,#1731);
#1330=LINE('',#7026,#1732);
#1331=LINE('',#7029,#1733);
#1332=LINE('',#7031,#1734);
#1333=LINE('',#7032,#1735);
#1334=LINE('',#7034,#1736);
#1335=LINE('',#7035,#1737);
#1336=LINE('',#7043,#1738);
#1337=LINE('',#7049,#1739);
#1338=LINE('',#7054,#1740);
#1339=LINE('',#7058,#1741);
#1340=LINE('',#7059,#1742);
#1341=LINE('',#7062,#1743);
#1342=LINE('',#7065,#1744);
#1343=LINE('',#7068,#1745);
#1344=LINE('',#7070,#1746);
#1345=LINE('',#7071,#1747);
#1346=LINE('',#7074,#1748);
#1347=LINE('',#7076,#1749);
#1348=LINE('',#7078,#1750);
#1349=LINE('',#7080,#1751);
#1350=LINE('',#7082,#1752);
#1351=LINE('',#7084,#1753);
#1352=LINE('',#7086,#1754);
#1353=LINE('',#7088,#1755);
#1354=LINE('',#7089,#1756);
#1355=LINE('',#7092,#1757);
#1356=LINE('',#7094,#1758);
#1357=LINE('',#7096,#1759);
#1358=LINE('',#7097,#1760);
#1359=LINE('',#7100,#1761);
#1360=LINE('',#7102,#1762);
#1361=LINE('',#7104,#1763);
#1362=LINE('',#7105,#1764);
#1363=LINE('',#7110,#1765);
#1364=LINE('',#7115,#1766);
#1365=LINE('',#7118,#1767);
#1366=LINE('',#7122,#1768);
#1367=LINE('',#7123,#1769);
#1368=LINE('',#7124,#1770);
#1369=LINE('',#7127,#1771);
#1370=LINE('',#7129,#1772);
#1371=LINE('',#7131,#1773);
#1372=LINE('',#7133,#1774);
#1373=LINE('',#7135,#1775);
#1374=LINE('',#7136,#1776);
#1375=LINE('',#7145,#1777);
#1376=LINE('',#7152,#1778);
#1377=LINE('',#7158,#1779);
#1378=LINE('',#7163,#1780);
#1379=LINE('',#7166,#1781);
#1380=LINE('',#7169,#1782);
#1381=LINE('',#7172,#1783);
#1382=LINE('',#7175,#1784);
#1383=LINE('',#7177,#1785);
#1384=LINE('',#7179,#1786);
#1385=LINE('',#7181,#1787);
#1386=LINE('',#7183,#1788);
#1387=LINE('',#7185,#1789);
#1388=LINE('',#7187,#1790);
#1389=LINE('',#7189,#1791);
#1390=LINE('',#7191,#1792);
#1391=LINE('',#7192,#1793);
#1392=LINE('',#7195,#1794);
#1393=LINE('',#7197,#1795);
#1394=LINE('',#7199,#1796);
#1395=LINE('',#7201,#1797);
#1396=LINE('',#7202,#1798);
#1397=LINE('',#7204,#1799);
#1398=LINE('',#7206,#1800);
#1399=LINE('',#7207,#1801);
#1400=LINE('',#7214,#1802);
#1401=LINE('',#7215,#1803);
#1402=LINE('',#7222,#1804);
#1403=LINE('',#7229,#1805);
#1404=LINE('',#7230,#1806);
#1405=LINE('',#7232,#1807);
#1406=LINE('',#7243,#1808);
#1407=LINE('',#7251,#1809);
#1408=LINE('',#7255,#1810);
#1409=LINE('',#7261,#1811);
#1410=LINE('',#7285,#1812);
#1411=LINE('',#7333,#1813);
#1412=LINE('',#7381,#1814);
#1413=LINE('',#7432,#1815);
#1414=LINE('',#7480,#1816);
#1415=LINE('',#7528,#1817);
#1416=LINE('',#7576,#1818);
#1417=LINE('',#7630,#1819);
#1418=LINE('',#7678,#1820);
#1419=LINE('',#7726,#1821);
#1420=LINE('',#7780,#1822);
#1421=LINE('',#7828,#1823);
#1422=LINE('',#7876,#1824);
#1423=LINE('',#7924,#1825);
#1424=LINE('',#7978,#1826);
#1425=LINE('',#8026,#1827);
#1426=LINE('',#8074,#1828);
#1427=LINE('',#8128,#1829);
#1428=LINE('',#8176,#1830);
#1429=LINE('',#8224,#1831);
#1430=LINE('',#8278,#1832);
#1431=LINE('',#8326,#1833);
#1432=LINE('',#8374,#1834);
#1433=LINE('',#8422,#1835);
#1434=LINE('',#8476,#1836);
#1435=LINE('',#8524,#1837);
#1436=LINE('',#8572,#1838);
#1437=LINE('',#8626,#1839);
#1438=LINE('',#8674,#1840);
#1439=LINE('',#8722,#1841);
#1440=LINE('',#8776,#1842);
#1441=LINE('',#8824,#1843);
#1442=LINE('',#8872,#1844);
#1443=LINE('',#8920,#1845);
#1444=LINE('',#8973,#1846);
#1445=LINE('',#8994,#1847);
#1446=LINE('',#9019,#1848);
#1447=LINE('',#9043,#1849);
#1448=LINE('',#9067,#1850);
#1449=LINE('',#9092,#1851);
#1450=LINE('',#9117,#1852);
#1451=LINE('',#9141,#1853);
#1452=LINE('',#9166,#1854);
#1453=LINE('',#9191,#1855);
#1454=LINE('',#9215,#1856);
#1455=LINE('',#9240,#1857);
#1456=LINE('',#9265,#1858);
#1457=LINE('',#9289,#1859);
#1458=LINE('',#9313,#1860);
#1459=LINE('',#9338,#1861);
#1460=LINE('',#9363,#1862);
#1461=LINE('',#9387,#1863);
#1462=LINE('',#9412,#1864);
#1463=LINE('',#9437,#1865);
#1464=LINE('',#9461,#1866);
#1465=LINE('',#9486,#1867);
#1466=LINE('',#9511,#1868);
#1467=LINE('',#9535,#1869);
#1468=LINE('',#9559,#1870);
#1469=LINE('',#9584,#1871);
#1470=LINE('',#9609,#1872);
#1471=LINE('',#9633,#1873);
#1472=LINE('',#9658,#1874);
#1473=LINE('',#9683,#1875);
#1474=LINE('',#9707,#1876);
#1475=LINE('',#9732,#1877);
#1476=LINE('',#9756,#1878);
#1477=LINE('',#9781,#1879);
#1478=LINE('',#11818,#1880);
#1479=LINE('',#11820,#1881);
#1480=LINE('',#11822,#1882);
#1481=LINE('',#11823,#1883);
#1482=LINE('',#11826,#1884);
#1483=LINE('',#11828,#1885);
#1484=LINE('',#11829,#1886);
#1485=LINE('',#11832,#1887);
#1486=LINE('',#11834,#1888);
#1487=LINE('',#11835,#1889);
#1488=LINE('',#11838,#1890);
#1489=LINE('',#11840,#1891);
#1490=LINE('',#11841,#1892);
#1491=LINE('',#11844,#1893);
#1492=LINE('',#11846,#1894);
#1493=LINE('',#11847,#1895);
#1494=LINE('',#11849,#1896);
#1495=LINE('',#11850,#1897);
#1496=LINE('',#11857,#1898);
#1497=LINE('',#11865,#1899);
#1498=LINE('',#11875,#1900);
#1499=LINE('',#11922,#1901);
#1500=LINE('',#11973,#1902);
#1501=LINE('',#12021,#1903);
#1502=LINE('',#12072,#1904);
#1503=LINE('',#12111,#1905);
#1504=LINE('',#12131,#1906);
#1505=LINE('',#12155,#1907);
#1506=LINE('',#12180,#1908);
#1507=LINE('',#12205,#1909);
#1508=LINE('',#12229,#1910);
#1509=LINE('',#12851,#1911);
#1510=LINE('',#12853,#1912);
#1511=LINE('',#12855,#1913);
#1512=LINE('',#12857,#1914);
#1513=LINE('',#12859,#1915);
#1514=LINE('',#12860,#1916);
#1515=LINE('',#12865,#1917);
#1516=LINE('',#12866,#1918);
#1517=LINE('',#12867,#1919);
#1518=LINE('',#12870,#1920);
#1519=LINE('',#12871,#1921);
#1520=LINE('',#12874,#1922);
#1521=LINE('',#12875,#1923);
#1522=LINE('',#12878,#1924);
#1523=LINE('',#12879,#1925);
#1524=LINE('',#12882,#1926);
#1525=LINE('',#12883,#1927);
#1526=LINE('',#12885,#1928);
#1527=LINE('',#12892,#1929);
#1528=VECTOR('',#5349,0.5);
#1529=VECTOR('',#5360,0.5);
#1530=VECTOR('',#5371,0.409999999999997);
#1531=VECTOR('',#5380,0.409999999999997);
#1532=VECTOR('',#5389,0.409999999999997);
#1533=VECTOR('',#5398,0.409999999999997);
#1534=VECTOR('',#5407,0.225000000000001);
#1535=VECTOR('',#5412,0.224999999999994);
#1536=VECTOR('',#5415,1.);
#1537=VECTOR('',#5416,1.);
#1538=VECTOR('',#5417,1.);
#1539=VECTOR('',#5418,1.);
#1540=VECTOR('',#5421,1.);
#1541=VECTOR('',#5422,1.);
#1542=VECTOR('',#5423,1.);
#1543=VECTOR('',#5424,1.);
#1544=VECTOR('',#5427,1.);
#1545=VECTOR('',#5428,1.);
#1546=VECTOR('',#5429,1.);
#1547=VECTOR('',#5430,1.);
#1548=VECTOR('',#5433,1.);
#1549=VECTOR('',#5434,1.);
#1550=VECTOR('',#5435,1.);
#1551=VECTOR('',#5436,1.);
#1552=VECTOR('',#5439,1.);
#1553=VECTOR('',#5440,1.);
#1554=VECTOR('',#5441,1.);
#1555=VECTOR('',#5442,1.);
#1556=VECTOR('',#5443,1.);
#1557=VECTOR('',#5444,1.);
#1558=VECTOR('',#5445,1.);
#1559=VECTOR('',#5446,1.);
#1560=VECTOR('',#5447,1.);
#1561=VECTOR('',#5448,1.);
#1562=VECTOR('',#5449,1.);
#1563=VECTOR('',#5450,1.);
#1564=VECTOR('',#5451,1.);
#1565=VECTOR('',#5452,1.);
#1566=VECTOR('',#5453,1.);
#1567=VECTOR('',#5454,1.);
#1568=VECTOR('',#5457,1.);
#1569=VECTOR('',#5458,1.);
#1570=VECTOR('',#5461,1.);
#1571=VECTOR('',#5462,1.);
#1572=VECTOR('',#5465,1.);
#1573=VECTOR('',#5466,1.);
#1574=VECTOR('',#5469,1.);
#1575=VECTOR('',#5470,1.);
#1576=VECTOR('',#5473,1.);
#1577=VECTOR('',#5476,1.);
#1578=VECTOR('',#5479,1.);
#1579=VECTOR('',#5480,1.);
#1580=VECTOR('',#5483,1.);
#1581=VECTOR('',#5484,1.);
#1582=VECTOR('',#5487,1.);
#1583=VECTOR('',#5488,1.);
#1584=VECTOR('',#5491,1.);
#1585=VECTOR('',#5492,1.);
#1586=VECTOR('',#5495,1.);
#1587=VECTOR('',#5498,1.);
#1588=VECTOR('',#5501,1.);
#1589=VECTOR('',#5502,1.);
#1590=VECTOR('',#5503,1.);
#1591=VECTOR('',#5506,1.);
#1592=VECTOR('',#5507,1.);
#1593=VECTOR('',#5510,1.);
#1594=VECTOR('',#5511,1.);
#1595=VECTOR('',#5514,1.);
#1596=VECTOR('',#5523,0.409999999999997);
#1597=VECTOR('',#5532,0.409999999999997);
#1598=VECTOR('',#5541,0.409999999999997);
#1599=VECTOR('',#5550,0.409999999999997);
#1600=VECTOR('',#5559,0.225000000000001);
#1601=VECTOR('',#5566,0.224999999999994);
#1602=VECTOR('',#5571,1.);
#1603=VECTOR('',#5572,1.);
#1604=VECTOR('',#5573,1.);
#1605=VECTOR('',#5574,1.);
#1606=VECTOR('',#5577,1.);
#1607=VECTOR('',#5578,1.);
#1608=VECTOR('',#5579,1.);
#1609=VECTOR('',#5580,1.);
#1610=VECTOR('',#5583,1.);
#1611=VECTOR('',#5584,1.);
#1612=VECTOR('',#5585,1.);
#1613=VECTOR('',#5586,1.);
#1614=VECTOR('',#5589,1.);
#1615=VECTOR('',#5590,1.);
#1616=VECTOR('',#5591,1.);
#1617=VECTOR('',#5592,1.);
#1618=VECTOR('',#5595,1.);
#1619=VECTOR('',#5596,1.);
#1620=VECTOR('',#5597,1.);
#1621=VECTOR('',#5598,1.);
#1622=VECTOR('',#5599,1.);
#1623=VECTOR('',#5600,1.);
#1624=VECTOR('',#5601,1.);
#1625=VECTOR('',#5602,1.);
#1626=VECTOR('',#5603,1.);
#1627=VECTOR('',#5604,1.);
#1628=VECTOR('',#5605,1.);
#1629=VECTOR('',#5606,1.);
#1630=VECTOR('',#5607,1.);
#1631=VECTOR('',#5608,1.);
#1632=VECTOR('',#5609,1.);
#1633=VECTOR('',#5610,1.);
#1634=VECTOR('',#5613,1.);
#1635=VECTOR('',#5614,1.);
#1636=VECTOR('',#5617,1.);
#1637=VECTOR('',#5618,1.);
#1638=VECTOR('',#5621,1.);
#1639=VECTOR('',#5622,1.);
#1640=VECTOR('',#5625,1.);
#1641=VECTOR('',#5626,1.);
#1642=VECTOR('',#5629,1.);
#1643=VECTOR('',#5632,1.);
#1644=VECTOR('',#5635,1.);
#1645=VECTOR('',#5636,1.);
#1646=VECTOR('',#5639,1.);
#1647=VECTOR('',#5640,1.);
#1648=VECTOR('',#5643,1.);
#1649=VECTOR('',#5644,1.);
#1650=VECTOR('',#5647,1.);
#1651=VECTOR('',#5648,1.);
#1652=VECTOR('',#5651,1.);
#1653=VECTOR('',#5654,1.);
#1654=VECTOR('',#5657,1.);
#1655=VECTOR('',#5658,1.);
#1656=VECTOR('',#5659,1.);
#1657=VECTOR('',#5662,1.);
#1658=VECTOR('',#5663,1.);
#1659=VECTOR('',#5666,1.);
#1660=VECTOR('',#5667,1.);
#1661=VECTOR('',#5670,1.);
#1662=VECTOR('',#5677,1.);
#1663=VECTOR('',#5678,1.);
#1664=VECTOR('',#5679,1.);
#1665=VECTOR('',#5680,1.);
#1666=VECTOR('',#5683,1.);
#1667=VECTOR('',#5684,1.);
#1668=VECTOR('',#5685,1.);
#1669=VECTOR('',#5686,1.);
#1670=VECTOR('',#5689,1.);
#1671=VECTOR('',#5690,1.);
#1672=VECTOR('',#5693,1.);
#1673=VECTOR('',#5694,1.);
#1674=VECTOR('',#5695,1.);
#1675=VECTOR('',#5696,1.);
#1676=VECTOR('',#5697,1.);
#1677=VECTOR('',#5700,1.);
#1678=VECTOR('',#5701,1.);
#1679=VECTOR('',#5704,1.);
#1680=VECTOR('',#5705,1.);
#1681=VECTOR('',#5706,1.);
#1682=VECTOR('',#5709,1.);
#1683=VECTOR('',#5710,1.);
#1684=VECTOR('',#5713,1.);
#1685=VECTOR('',#5714,1.);
#1686=VECTOR('',#5723,1.);
#1687=VECTOR('',#5724,1.);
#1688=VECTOR('',#5725,1.);
#1689=VECTOR('',#5726,1.);
#1690=VECTOR('',#5729,1.);
#1691=VECTOR('',#5730,1.);
#1692=VECTOR('',#5731,1.);
#1693=VECTOR('',#5734,1.);
#1694=VECTOR('',#5735,1.);
#1695=VECTOR('',#5736,1.);
#1696=VECTOR('',#5739,1.);
#1697=VECTOR('',#5740,1.);
#1698=VECTOR('',#5749,1.);
#1699=VECTOR('',#5750,1.);
#1700=VECTOR('',#5751,1.);
#1701=VECTOR('',#5752,1.);
#1702=VECTOR('',#5755,1.);
#1703=VECTOR('',#5756,1.);
#1704=VECTOR('',#5757,1.);
#1705=VECTOR('',#5760,1.);
#1706=VECTOR('',#5761,1.);
#1707=VECTOR('',#5762,1.);
#1708=VECTOR('',#5765,1.);
#1709=VECTOR('',#5766,1.);
#1710=VECTOR('',#5767,1.);
#1711=VECTOR('',#5770,1.);
#1712=VECTOR('',#5771,1.);
#1713=VECTOR('',#5772,1.);
#1714=VECTOR('',#5775,1.);
#1715=VECTOR('',#5776,1.);
#1716=VECTOR('',#5785,1.);
#1717=VECTOR('',#5786,1.);
#1718=VECTOR('',#5787,1.);
#1719=VECTOR('',#5788,1.);
#1720=VECTOR('',#5793,1.);
#1721=VECTOR('',#5798,1.);
#1722=VECTOR('',#5799,1.);
#1723=VECTOR('',#5800,1.);
#1724=VECTOR('',#5811,0.225);
#1725=VECTOR('',#5818,0.225);
#1726=VECTOR('',#5823,1.);
#1727=VECTOR('',#5824,1.);
#1728=VECTOR('',#5825,1.);
#1729=VECTOR('',#5826,1.);
#1730=VECTOR('',#5829,1.);
#1731=VECTOR('',#5830,1.);
#1732=VECTOR('',#5831,1.);
#1733=VECTOR('',#5834,1.);
#1734=VECTOR('',#5835,1.);
#1735=VECTOR('',#5836,1.);
#1736=VECTOR('',#5839,1.);
#1737=VECTOR('',#5840,1.);
#1738=VECTOR('',#5851,0.225000000000001);
#1739=VECTOR('',#5858,0.224999999999994);
#1740=VECTOR('',#5863,1.);
#1741=VECTOR('',#5866,1.);
#1742=VECTOR('',#5867,1.);
#1743=VECTOR('',#5870,1.);
#1744=VECTOR('',#5873,1.);
#1745=VECTOR('',#5876,1.);
#1746=VECTOR('',#5877,1.);
#1747=VECTOR('',#5878,1.);
#1748=VECTOR('',#5881,1.);
#1749=VECTOR('',#5882,1.);
#1750=VECTOR('',#5883,1.);
#1751=VECTOR('',#5884,1.);
#1752=VECTOR('',#5885,1.);
#1753=VECTOR('',#5886,1.);
#1754=VECTOR('',#5887,1.);
#1755=VECTOR('',#5888,1.);
#1756=VECTOR('',#5889,1.);
#1757=VECTOR('',#5892,1.);
#1758=VECTOR('',#5893,1.);
#1759=VECTOR('',#5894,1.);
#1760=VECTOR('',#5895,1.);
#1761=VECTOR('',#5898,1.);
#1762=VECTOR('',#5899,1.);
#1763=VECTOR('',#5900,1.);
#1764=VECTOR('',#5901,1.);
#1765=VECTOR('',#5906,1.);
#1766=VECTOR('',#5913,1.);
#1767=VECTOR('',#5916,1.);
#1768=VECTOR('',#5921,1.);
#1769=VECTOR('',#5922,1.);
#1770=VECTOR('',#5923,1.);
#1771=VECTOR('',#5926,1.);
#1772=VECTOR('',#5927,1.);
#1773=VECTOR('',#5928,1.);
#1774=VECTOR('',#5929,1.);
#1775=VECTOR('',#5930,1.);
#1776=VECTOR('',#5931,1.);
#1777=VECTOR('',#5948,1.);
#1778=VECTOR('',#5957,0.225);
#1779=VECTOR('',#5964,0.225);
#1780=VECTOR('',#5969,1.);
#1781=VECTOR('',#5972,1.);
#1782=VECTOR('',#5975,1.);
#1783=VECTOR('',#5978,1.);
#1784=VECTOR('',#5981,1.);
#1785=VECTOR('',#5982,1.);
#1786=VECTOR('',#5983,1.);
#1787=VECTOR('',#5984,1.);
#1788=VECTOR('',#5985,1.);
#1789=VECTOR('',#5986,1.);
#1790=VECTOR('',#5987,1.);
#1791=VECTOR('',#5988,1.);
#1792=VECTOR('',#5989,1.);
#1793=VECTOR('',#5990,1.);
#1794=VECTOR('',#5993,1.);
#1795=VECTOR('',#5994,1.);
#1796=VECTOR('',#5995,1.);
#1797=VECTOR('',#5996,1.);
#1798=VECTOR('',#5997,1.);
#1799=VECTOR('',#5998,1.);
#1800=VECTOR('',#5999,1.);
#1801=VECTOR('',#6000,1.);
#1802=VECTOR('',#6011,1.);
#1803=VECTOR('',#6012,1.);
#1804=VECTOR('',#6021,0.22);
#1805=VECTOR('',#6032,1.);
#1806=VECTOR('',#6033,1.);
#1807=VECTOR('',#6036,1.);
#1808=VECTOR('',#6051,0.3);
#1809=VECTOR('',#6060,0.35);
#1810=VECTOR('',#6067,0.2);
#1811=VECTOR('',#6074,0.2);
#1812=VECTOR('',#6079,0.2);
#1813=VECTOR('',#6082,0.2);
#1814=VECTOR('',#6085,0.2);
#1815=VECTOR('',#6088,0.2);
#1816=VECTOR('',#6091,0.2);
#1817=VECTOR('',#6094,0.2);
#1818=VECTOR('',#6097,0.2);
#1819=VECTOR('',#6100,0.2);
#1820=VECTOR('',#6103,0.2);
#1821=VECTOR('',#6106,0.2);
#1822=VECTOR('',#6109,0.2);
#1823=VECTOR('',#6112,0.2);
#1824=VECTOR('',#6115,0.2);
#1825=VECTOR('',#6118,0.2);
#1826=VECTOR('',#6121,0.2);
#1827=VECTOR('',#6124,0.2);
#1828=VECTOR('',#6127,0.2);
#1829=VECTOR('',#6130,0.2);
#1830=VECTOR('',#6133,0.2);
#1831=VECTOR('',#6136,0.2);
#1832=VECTOR('',#6139,0.2);
#1833=VECTOR('',#6142,0.2);
#1834=VECTOR('',#6145,0.2);
#1835=VECTOR('',#6148,0.2);
#1836=VECTOR('',#6151,0.2);
#1837=VECTOR('',#6154,0.2);
#1838=VECTOR('',#6157,0.2);
#1839=VECTOR('',#6160,0.2);
#1840=VECTOR('',#6163,0.2);
#1841=VECTOR('',#6166,0.2);
#1842=VECTOR('',#6169,0.2);
#1843=VECTOR('',#6172,0.2);
#1844=VECTOR('',#6175,0.2);
#1845=VECTOR('',#6178,0.2);
#1846=VECTOR('',#6183,0.15555);
#1847=VECTOR('',#6188,0.15555);
#1848=VECTOR('',#6191,0.15555);
#1849=VECTOR('',#6194,0.15555);
#1850=VECTOR('',#6197,0.15555);
#1851=VECTOR('',#6200,0.15555);
#1852=VECTOR('',#6203,0.15555);
#1853=VECTOR('',#6206,0.15555);
#1854=VECTOR('',#6209,0.15555);
#1855=VECTOR('',#6212,0.15555);
#1856=VECTOR('',#6215,0.15555);
#1857=VECTOR('',#6218,0.15555);
#1858=VECTOR('',#6221,0.15555);
#1859=VECTOR('',#6224,0.15555);
#1860=VECTOR('',#6227,0.15555);
#1861=VECTOR('',#6230,0.15555);
#1862=VECTOR('',#6233,0.15555);
#1863=VECTOR('',#6236,0.15555);
#1864=VECTOR('',#6239,0.15555);
#1865=VECTOR('',#6242,0.15555);
#1866=VECTOR('',#6245,0.15555);
#1867=VECTOR('',#6248,0.15555);
#1868=VECTOR('',#6251,0.15555);
#1869=VECTOR('',#6254,0.15555);
#1870=VECTOR('',#6257,0.15555);
#1871=VECTOR('',#6260,0.15555);
#1872=VECTOR('',#6263,0.15555);
#1873=VECTOR('',#6266,0.15555);
#1874=VECTOR('',#6269,0.15555);
#1875=VECTOR('',#6272,0.15555);
#1876=VECTOR('',#6275,0.15555);
#1877=VECTOR('',#6278,0.15555);
#1878=VECTOR('',#6281,0.15555);
#1879=VECTOR('',#6284,0.15555);
#1880=VECTOR('',#6295,1.);
#1881=VECTOR('',#6296,1.);
#1882=VECTOR('',#6297,1.);
#1883=VECTOR('',#6298,1.);
#1884=VECTOR('',#6301,1.);
#1885=VECTOR('',#6302,1.);
#1886=VECTOR('',#6303,1.);
#1887=VECTOR('',#6306,1.);
#1888=VECTOR('',#6307,1.);
#1889=VECTOR('',#6308,1.);
#1890=VECTOR('',#6311,1.);
#1891=VECTOR('',#6312,1.);
#1892=VECTOR('',#6313,1.);
#1893=VECTOR('',#6316,1.);
#1894=VECTOR('',#6317,1.);
#1895=VECTOR('',#6318,1.);
#1896=VECTOR('',#6321,1.);
#1897=VECTOR('',#6322,1.);
#1898=VECTOR('',#6331,0.4);
#1899=VECTOR('',#6342,0.2);
#1900=VECTOR('',#6347,0.2);
#1901=VECTOR('',#6352,0.2);
#1902=VECTOR('',#6355,0.2);
#1903=VECTOR('',#6358,0.2);
#1904=VECTOR('',#6361,0.2);
#1905=VECTOR('',#6366,0.205475);
#1906=VECTOR('',#6371,0.205475);
#1907=VECTOR('',#6374,0.205475);
#1908=VECTOR('',#6377,0.205475);
#1909=VECTOR('',#6380,0.205475);
#1910=VECTOR('',#6383,0.205475);
#1911=VECTOR('',#6390,1.);
#1912=VECTOR('',#6391,1.);
#1913=VECTOR('',#6392,1.);
#1914=VECTOR('',#6393,1.);
#1915=VECTOR('',#6394,1.);
#1916=VECTOR('',#6395,1.);
#1917=VECTOR('',#6400,1.);
#1918=VECTOR('',#6401,1.);
#1919=VECTOR('',#6402,1.);
#1920=VECTOR('',#6405,1.);
#1921=VECTOR('',#6406,1.);
#1922=VECTOR('',#6409,1.);
#1923=VECTOR('',#6410,1.);
#1924=VECTOR('',#6413,1.);
#1925=VECTOR('',#6414,1.);
#1926=VECTOR('',#6417,1.);
#1927=VECTOR('',#6418,1.);
#1928=VECTOR('',#6421,1.);
#1929=VECTOR('',#6430,0.4);
#1930=CIRCLE('',#4957,0.5);
#1931=CIRCLE('',#4958,0.5);
#1932=CIRCLE('',#4960,0.225000000000001);
#1933=CIRCLE('',#4962,0.5);
#1934=CIRCLE('',#4963,0.5);
#1935=CIRCLE('',#4965,0.224999999999994);
#1936=CIRCLE('',#4967,0.409999999999997);
#1937=CIRCLE('',#4968,0.409999999999997);
#1938=CIRCLE('',#4971,0.409999999999997);
#1939=CIRCLE('',#4972,0.409999999999997);
#1940=CIRCLE('',#4975,0.409999999999997);
#1941=CIRCLE('',#4976,0.409999999999997);
#1942=CIRCLE('',#4979,0.409999999999997);
#1943=CIRCLE('',#4980,0.409999999999997);
#1944=CIRCLE('',#4983,0.225000000000001);
#1945=CIRCLE('',#4985,0.224999999999994);
#1946=CIRCLE('',#5010,0.409999999999997);
#1947=CIRCLE('',#5011,0.409999999999997);
#1948=CIRCLE('',#5014,0.409999999999997);
#1949=CIRCLE('',#5015,0.409999999999997);
#1950=CIRCLE('',#5018,0.409999999999997);
#1951=CIRCLE('',#5019,0.409999999999997);
#1952=CIRCLE('',#5022,0.409999999999997);
#1953=CIRCLE('',#5023,0.409999999999997);
#1954=CIRCLE('',#5026,0.225000000000001);
#1955=CIRCLE('',#5027,0.225000000000001);
#1956=CIRCLE('',#5029,0.224999999999994);
#1957=CIRCLE('',#5030,0.224999999999994);
#1958=CIRCLE('',#5083,1.);
#1959=CIRCLE('',#5084,1.);
#1960=CIRCLE('',#5087,1.);
#1961=CIRCLE('',#5088,1.);
#1962=CIRCLE('',#5090,0.225);
#1963=CIRCLE('',#5091,0.225);
#1964=CIRCLE('',#5093,0.225);
#1965=CIRCLE('',#5094,0.225);
#1966=CIRCLE('',#5103,0.225000000000001);
#1967=CIRCLE('',#5104,0.225000000000001);
#1968=CIRCLE('',#5106,0.224999999999994);
#1969=CIRCLE('',#5107,0.224999999999994);
#1970=CIRCLE('',#5109,0.42);
#1971=CIRCLE('',#5111,0.42);
#1972=CIRCLE('',#5117,0.4);
#1973=CIRCLE('',#5118,0.22);
#1974=CIRCLE('',#5120,0.4);
#1975=CIRCLE('',#5122,0.22);
#1976=CIRCLE('',#5126,0.22);
#1977=CIRCLE('',#5127,0.22);
#1978=CIRCLE('',#5129,0.4);
#1979=CIRCLE('',#5130,0.4);
#1980=CIRCLE('',#5136,0.225);
#1981=CIRCLE('',#5137,0.225);
#1982=CIRCLE('',#5139,0.225);
#1983=CIRCLE('',#5140,0.225);
#1984=CIRCLE('',#5142,0.42);
#1985=CIRCLE('',#5144,0.42);
#1986=CIRCLE('',#5148,0.42);
#1987=CIRCLE('',#5149,0.42);
#1988=CIRCLE('',#5153,0.4);
#1989=CIRCLE('',#5154,0.22);
#1990=CIRCLE('',#5156,0.22);
#1991=CIRCLE('',#5158,0.4);
#1992=CIRCLE('',#5165,0.3);
#1993=CIRCLE('',#5166,0.2);
#1994=CIRCLE('',#5168,0.3);
#1995=CIRCLE('',#5170,0.35);
#1996=CIRCLE('',#5171,0.2);
#1997=CIRCLE('',#5173,0.35);
#1998=CIRCLE('',#5179,0.1954);
#1999=CIRCLE('',#5214,0.1954);
#2000=CIRCLE('',#5216,0.15555);
#2001=CIRCLE('',#5251,0.15555);
#2002=CIRCLE('',#5253,0.1954);
#2003=CIRCLE('',#5262,0.4);
#2004=CIRCLE('',#5264,0.4);
#2005=CIRCLE('',#5269,0.1666);
#2006=CIRCLE('',#5271,0.1666);
#2007=CIRCLE('',#5276,0.1666);
#2008=CIRCLE('',#5278,0.205475);
#2009=CIRCLE('',#5284,0.205475);
#2010=CIRCLE('',#5297,0.4);
#2011=CIRCLE('',#5298,0.4);
#2012=VERTEX_POINT('',#6520);
#2013=VERTEX_POINT('',#6522);
#2014=VERTEX_POINT('',#6526);
#2015=VERTEX_POINT('',#6529);
#2016=VERTEX_POINT('',#6531);
#2017=VERTEX_POINT('',#6535);
#2018=VERTEX_POINT('',#6538);
#2019=VERTEX_POINT('',#6540);
#2020=VERTEX_POINT('',#6545);
#2021=VERTEX_POINT('',#6547);
#2022=VERTEX_POINT('',#6552);
#2023=VERTEX_POINT('',#6554);
#2024=VERTEX_POINT('',#6559);
#2025=VERTEX_POINT('',#6561);
#2026=VERTEX_POINT('',#6566);
#2027=VERTEX_POINT('',#6570);
#2028=VERTEX_POINT('',#6574);
#2029=VERTEX_POINT('',#6575);
#2030=VERTEX_POINT('',#6577);
#2031=VERTEX_POINT('',#6579);
#2032=VERTEX_POINT('',#6583);
#2033=VERTEX_POINT('',#6584);
#2034=VERTEX_POINT('',#6586);
#2035=VERTEX_POINT('',#6588);
#2036=VERTEX_POINT('',#6592);
#2037=VERTEX_POINT('',#6593);
#2038=VERTEX_POINT('',#6595);
#2039=VERTEX_POINT('',#6597);
#2040=VERTEX_POINT('',#6601);
#2041=VERTEX_POINT('',#6602);
#2042=VERTEX_POINT('',#6604);
#2043=VERTEX_POINT('',#6606);
#2044=VERTEX_POINT('',#6610);
#2045=VERTEX_POINT('',#6612);
#2046=VERTEX_POINT('',#6614);
#2047=VERTEX_POINT('',#6616);
#2048=VERTEX_POINT('',#6619);
#2049=VERTEX_POINT('',#6621);
#2050=VERTEX_POINT('',#6624);
#2051=VERTEX_POINT('',#6626);
#2052=VERTEX_POINT('',#6628);
#2053=VERTEX_POINT('',#6630);
#2054=VERTEX_POINT('',#6633);
#2055=VERTEX_POINT('',#6635);
#2056=VERTEX_POINT('',#6639);
#2057=VERTEX_POINT('',#6643);
#2058=VERTEX_POINT('',#6647);
#2059=VERTEX_POINT('',#6651);
#2060=VERTEX_POINT('',#6659);
#2061=VERTEX_POINT('',#6663);
#2062=VERTEX_POINT('',#6667);
#2063=VERTEX_POINT('',#6671);
#2064=VERTEX_POINT('',#6679);
#2065=VERTEX_POINT('',#6681);
#2066=VERTEX_POINT('',#6685);
#2067=VERTEX_POINT('',#6689);
#2068=VERTEX_POINT('',#6697);
#2069=VERTEX_POINT('',#6699);
#2070=VERTEX_POINT('',#6704);
#2071=VERTEX_POINT('',#6706);
#2072=VERTEX_POINT('',#6711);
#2073=VERTEX_POINT('',#6713);
#2074=VERTEX_POINT('',#6718);
#2075=VERTEX_POINT('',#6720);
#2076=VERTEX_POINT('',#6725);
#2077=VERTEX_POINT('',#6727);
#2078=VERTEX_POINT('',#6731);
#2079=VERTEX_POINT('',#6733);
#2080=VERTEX_POINT('',#6737);
#2081=VERTEX_POINT('',#6738);
#2082=VERTEX_POINT('',#6740);
#2083=VERTEX_POINT('',#6742);
#2084=VERTEX_POINT('',#6746);
#2085=VERTEX_POINT('',#6747);
#2086=VERTEX_POINT('',#6749);
#2087=VERTEX_POINT('',#6751);
#2088=VERTEX_POINT('',#6755);
#2089=VERTEX_POINT('',#6756);
#2090=VERTEX_POINT('',#6758);
#2091=VERTEX_POINT('',#6760);
#2092=VERTEX_POINT('',#6764);
#2093=VERTEX_POINT('',#6765);
#2094=VERTEX_POINT('',#6767);
#2095=VERTEX_POINT('',#6769);
#2096=VERTEX_POINT('',#6773);
#2097=VERTEX_POINT('',#6775);
#2098=VERTEX_POINT('',#6777);
#2099=VERTEX_POINT('',#6779);
#2100=VERTEX_POINT('',#6782);
#2101=VERTEX_POINT('',#6784);
#2102=VERTEX_POINT('',#6787);
#2103=VERTEX_POINT('',#6789);
#2104=VERTEX_POINT('',#6791);
#2105=VERTEX_POINT('',#6793);
#2106=VERTEX_POINT('',#6796);
#2107=VERTEX_POINT('',#6798);
#2108=VERTEX_POINT('',#6802);
#2109=VERTEX_POINT('',#6806);
#2110=VERTEX_POINT('',#6810);
#2111=VERTEX_POINT('',#6814);
#2112=VERTEX_POINT('',#6822);
#2113=VERTEX_POINT('',#6826);
#2114=VERTEX_POINT('',#6830);
#2115=VERTEX_POINT('',#6834);
#2116=VERTEX_POINT('',#6842);
#2117=VERTEX_POINT('',#6844);
#2118=VERTEX_POINT('',#6848);
#2119=VERTEX_POINT('',#6852);
#2120=VERTEX_POINT('',#6860);
#2121=VERTEX_POINT('',#6861);
#2122=VERTEX_POINT('',#6863);
#2123=VERTEX_POINT('',#6865);
#2124=VERTEX_POINT('',#6869);
#2125=VERTEX_POINT('',#6870);
#2126=VERTEX_POINT('',#6872);
#2127=VERTEX_POINT('',#6874);
#2128=VERTEX_POINT('',#6881);
#2129=VERTEX_POINT('',#6883);
#2130=VERTEX_POINT('',#6885);
#2131=VERTEX_POINT('',#6887);
#2132=VERTEX_POINT('',#6891);
#2133=VERTEX_POINT('',#6895);
#2134=VERTEX_POINT('',#6897);
#2135=VERTEX_POINT('',#6901);
#2136=VERTEX_POINT('',#6911);
#2137=VERTEX_POINT('',#6912);
#2138=VERTEX_POINT('',#6914);
#2139=VERTEX_POINT('',#6916);
#2140=VERTEX_POINT('',#6920);
#2141=VERTEX_POINT('',#6922);
#2142=VERTEX_POINT('',#6926);
#2143=VERTEX_POINT('',#6928);
#2144=VERTEX_POINT('',#6938);
#2145=VERTEX_POINT('',#6939);
#2146=VERTEX_POINT('',#6941);
#2147=VERTEX_POINT('',#6943);
#2148=VERTEX_POINT('',#6947);
#2149=VERTEX_POINT('',#6949);
#2150=VERTEX_POINT('',#6953);
#2151=VERTEX_POINT('',#6955);
#2152=VERTEX_POINT('',#6959);
#2153=VERTEX_POINT('',#6961);
#2154=VERTEX_POINT('',#6965);
#2155=VERTEX_POINT('',#6967);
#2156=VERTEX_POINT('',#6977);
#2157=VERTEX_POINT('',#6978);
#2158=VERTEX_POINT('',#6980);
#2159=VERTEX_POINT('',#6982);
#2160=VERTEX_POINT('',#6986);
#2161=VERTEX_POINT('',#6988);
#2162=VERTEX_POINT('',#6992);
#2163=VERTEX_POINT('',#6994);
#2164=VERTEX_POINT('',#7001);
#2165=VERTEX_POINT('',#7003);
#2166=VERTEX_POINT('',#7007);
#2167=VERTEX_POINT('',#7009);
#2168=VERTEX_POINT('',#7013);
#2169=VERTEX_POINT('',#7014);
#2170=VERTEX_POINT('',#7016);
#2171=VERTEX_POINT('',#7018);
#2172=VERTEX_POINT('',#7022);
#2173=VERTEX_POINT('',#7024);
#2174=VERTEX_POINT('',#7028);
#2175=VERTEX_POINT('',#7030);
#2176=VERTEX_POINT('',#7040);
#2177=VERTEX_POINT('',#7042);
#2178=VERTEX_POINT('',#7046);
#2179=VERTEX_POINT('',#7048);
#2180=VERTEX_POINT('',#7052);
#2181=VERTEX_POINT('',#7053);
#2182=VERTEX_POINT('',#7055);
#2183=VERTEX_POINT('',#7057);
#2184=VERTEX_POINT('',#7061);
#2185=VERTEX_POINT('',#7063);
#2186=VERTEX_POINT('',#7067);
#2187=VERTEX_POINT('',#7069);
#2188=VERTEX_POINT('',#7073);
#2189=VERTEX_POINT('',#7075);
#2190=VERTEX_POINT('',#7077);
#2191=VERTEX_POINT('',#7079);
#2192=VERTEX_POINT('',#7081);
#2193=VERTEX_POINT('',#7083);
#2194=VERTEX_POINT('',#7085);
#2195=VERTEX_POINT('',#7087);
#2196=VERTEX_POINT('',#7091);
#2197=VERTEX_POINT('',#7093);
#2198=VERTEX_POINT('',#7095);
#2199=VERTEX_POINT('',#7099);
#2200=VERTEX_POINT('',#7101);
#2201=VERTEX_POINT('',#7103);
#2202=VERTEX_POINT('',#7107);
#2203=VERTEX_POINT('',#7109);
#2204=VERTEX_POINT('',#7113);
#2205=VERTEX_POINT('',#7117);
#2206=VERTEX_POINT('',#7121);
#2207=VERTEX_POINT('',#7126);
#2208=VERTEX_POINT('',#7128);
#2209=VERTEX_POINT('',#7130);
#2210=VERTEX_POINT('',#7132);
#2211=VERTEX_POINT('',#7134);
#2212=VERTEX_POINT('',#7149);
#2213=VERTEX_POINT('',#7151);
#2214=VERTEX_POINT('',#7155);
#2215=VERTEX_POINT('',#7157);
#2216=VERTEX_POINT('',#7161);
#2217=VERTEX_POINT('',#7162);
#2218=VERTEX_POINT('',#7164);
#2219=VERTEX_POINT('',#7168);
#2220=VERTEX_POINT('',#7170);
#2221=VERTEX_POINT('',#7174);
#2222=VERTEX_POINT('',#7176);
#2223=VERTEX_POINT('',#7178);
#2224=VERTEX_POINT('',#7180);
#2225=VERTEX_POINT('',#7182);
#2226=VERTEX_POINT('',#7184);
#2227=VERTEX_POINT('',#7186);
#2228=VERTEX_POINT('',#7188);
#2229=VERTEX_POINT('',#7190);
#2230=VERTEX_POINT('',#7194);
#2231=VERTEX_POINT('',#7196);
#2232=VERTEX_POINT('',#7198);
#2233=VERTEX_POINT('',#7200);
#2234=VERTEX_POINT('',#7203);
#2235=VERTEX_POINT('',#7205);
#2236=VERTEX_POINT('',#7213);
#2237=VERTEX_POINT('',#7218);
#2238=VERTEX_POINT('',#7221);
#2239=VERTEX_POINT('',#7228);
#2240=VERTEX_POINT('',#7236);
#2241=VERTEX_POINT('',#7238);
#2242=VERTEX_POINT('',#7241);
#2243=VERTEX_POINT('',#7245);
#2244=VERTEX_POINT('',#7247);
#2245=VERTEX_POINT('',#7250);
#2246=VERTEX_POINT('',#7259);
#2247=VERTEX_POINT('',#7260);
#2248=VERTEX_POINT('',#7262);
#2249=VERTEX_POINT('',#7273);
#2250=VERTEX_POINT('',#7283);
#2251=VERTEX_POINT('',#7284);
#2252=VERTEX_POINT('',#7331);
#2253=VERTEX_POINT('',#7332);
#2254=VERTEX_POINT('',#7379);
#2255=VERTEX_POINT('',#7380);
#2256=VERTEX_POINT('',#7430);
#2257=VERTEX_POINT('',#7431);
#2258=VERTEX_POINT('',#7478);
#2259=VERTEX_POINT('',#7479);
#2260=VERTEX_POINT('',#7526);
#2261=VERTEX_POINT('',#7527);
#2262=VERTEX_POINT('',#7574);
#2263=VERTEX_POINT('',#7575);
#2264=VERTEX_POINT('',#7628);
#2265=VERTEX_POINT('',#7629);
#2266=VERTEX_POINT('',#7676);
#2267=VERTEX_POINT('',#7677);
#2268=VERTEX_POINT('',#7724);
#2269=VERTEX_POINT('',#7725);
#2270=VERTEX_POINT('',#7778);
#2271=VERTEX_POINT('',#7779);
#2272=VERTEX_POINT('',#7826);
#2273=VERTEX_POINT('',#7827);
#2274=VERTEX_POINT('',#7874);
#2275=VERTEX_POINT('',#7875);
#2276=VERTEX_POINT('',#7922);
#2277=VERTEX_POINT('',#7923);
#2278=VERTEX_POINT('',#7976);
#2279=VERTEX_POINT('',#7977);
#2280=VERTEX_POINT('',#8024);
#2281=VERTEX_POINT('',#8025);
#2282=VERTEX_POINT('',#8072);
#2283=VERTEX_POINT('',#8073);
#2284=VERTEX_POINT('',#8126);
#2285=VERTEX_POINT('',#8127);
#2286=VERTEX_POINT('',#8174);
#2287=VERTEX_POINT('',#8175);
#2288=VERTEX_POINT('',#8222);
#2289=VERTEX_POINT('',#8223);
#2290=VERTEX_POINT('',#8276);
#2291=VERTEX_POINT('',#8277);
#2292=VERTEX_POINT('',#8324);
#2293=VERTEX_POINT('',#8325);
#2294=VERTEX_POINT('',#8372);
#2295=VERTEX_POINT('',#8373);
#2296=VERTEX_POINT('',#8420);
#2297=VERTEX_POINT('',#8421);
#2298=VERTEX_POINT('',#8474);
#2299=VERTEX_POINT('',#8475);
#2300=VERTEX_POINT('',#8522);
#2301=VERTEX_POINT('',#8523);
#2302=VERTEX_POINT('',#8570);
#2303=VERTEX_POINT('',#8571);
#2304=VERTEX_POINT('',#8624);
#2305=VERTEX_POINT('',#8625);
#2306=VERTEX_POINT('',#8672);
#2307=VERTEX_POINT('',#8673);
#2308=VERTEX_POINT('',#8720);
#2309=VERTEX_POINT('',#8721);
#2310=VERTEX_POINT('',#8774);
#2311=VERTEX_POINT('',#8775);
#2312=VERTEX_POINT('',#8822);
#2313=VERTEX_POINT('',#8823);
#2314=VERTEX_POINT('',#8870);
#2315=VERTEX_POINT('',#8871);
#2316=VERTEX_POINT('',#8918);
#2317=VERTEX_POINT('',#8919);
#2318=VERTEX_POINT('',#8921);
#2319=VERTEX_POINT('',#8971);
#2320=VERTEX_POINT('',#8972);
#2321=VERTEX_POINT('',#8974);
#2322=VERTEX_POINT('',#8983);
#2323=VERTEX_POINT('',#8992);
#2324=VERTEX_POINT('',#8993);
#2325=VERTEX_POINT('',#9017);
#2326=VERTEX_POINT('',#9018);
#2327=VERTEX_POINT('',#9041);
#2328=VERTEX_POINT('',#9042);
#2329=VERTEX_POINT('',#9065);
#2330=VERTEX_POINT('',#9066);
#2331=VERTEX_POINT('',#9090);
#2332=VERTEX_POINT('',#9091);
#2333=VERTEX_POINT('',#9115);
#2334=VERTEX_POINT('',#9116);
#2335=VERTEX_POINT('',#9139);
#2336=VERTEX_POINT('',#9140);
#2337=VERTEX_POINT('',#9164);
#2338=VERTEX_POINT('',#9165);
#2339=VERTEX_POINT('',#9189);
#2340=VERTEX_POINT('',#9190);
#2341=VERTEX_POINT('',#9213);
#2342=VERTEX_POINT('',#9214);
#2343=VERTEX_POINT('',#9238);
#2344=VERTEX_POINT('',#9239);
#2345=VERTEX_POINT('',#9263);
#2346=VERTEX_POINT('',#9264);
#2347=VERTEX_POINT('',#9287);
#2348=VERTEX_POINT('',#9288);
#2349=VERTEX_POINT('',#9311);
#2350=VERTEX_POINT('',#9312);
#2351=VERTEX_POINT('',#9336);
#2352=VERTEX_POINT('',#9337);
#2353=VERTEX_POINT('',#9361);
#2354=VERTEX_POINT('',#9362);
#2355=VERTEX_POINT('',#9385);
#2356=VERTEX_POINT('',#9386);
#2357=VERTEX_POINT('',#9410);
#2358=VERTEX_POINT('',#9411);
#2359=VERTEX_POINT('',#9435);
#2360=VERTEX_POINT('',#9436);
#2361=VERTEX_POINT('',#9459);
#2362=VERTEX_POINT('',#9460);
#2363=VERTEX_POINT('',#9484);
#2364=VERTEX_POINT('',#9485);
#2365=VERTEX_POINT('',#9509);
#2366=VERTEX_POINT('',#9510);
#2367=VERTEX_POINT('',#9533);
#2368=VERTEX_POINT('',#9534);
#2369=VERTEX_POINT('',#9557);
#2370=VERTEX_POINT('',#9558);
#2371=VERTEX_POINT('',#9582);
#2372=VERTEX_POINT('',#9583);
#2373=VERTEX_POINT('',#9607);
#2374=VERTEX_POINT('',#9608);
#2375=VERTEX_POINT('',#9631);
#2376=VERTEX_POINT('',#9632);
#2377=VERTEX_POINT('',#9656);
#2378=VERTEX_POINT('',#9657);
#2379=VERTEX_POINT('',#9681);
#2380=VERTEX_POINT('',#9682);
#2381=VERTEX_POINT('',#9705);
#2382=VERTEX_POINT('',#9706);
#2383=VERTEX_POINT('',#9730);
#2384=VERTEX_POINT('',#9731);
#2385=VERTEX_POINT('',#9754);
#2386=VERTEX_POINT('',#9755);
#2387=VERTEX_POINT('',#9779);
#2388=VERTEX_POINT('',#9780);
#2389=VERTEX_POINT('',#10686);
#2390=VERTEX_POINT('',#10746);
#2391=VERTEX_POINT('',#10809);
#2392=VERTEX_POINT('',#11816);
#2393=VERTEX_POINT('',#11817);
#2394=VERTEX_POINT('',#11819);
#2395=VERTEX_POINT('',#11821);
#2396=VERTEX_POINT('',#11825);
#2397=VERTEX_POINT('',#11827);
#2398=VERTEX_POINT('',#11831);
#2399=VERTEX_POINT('',#11833);
#2400=VERTEX_POINT('',#11837);
#2401=VERTEX_POINT('',#11839);
#2402=VERTEX_POINT('',#11843);
#2403=VERTEX_POINT('',#11845);
#2404=VERTEX_POINT('',#11853);
#2405=VERTEX_POINT('',#11856);
#2406=VERTEX_POINT('',#11863);
#2407=VERTEX_POINT('',#11864);
#2408=VERTEX_POINT('',#11866);
#2409=VERTEX_POINT('',#11873);
#2410=VERTEX_POINT('',#11874);
#2411=VERTEX_POINT('',#11876);
#2412=VERTEX_POINT('',#11920);
#2413=VERTEX_POINT('',#11921);
#2414=VERTEX_POINT('',#11971);
#2415=VERTEX_POINT('',#11972);
#2416=VERTEX_POINT('',#12019);
#2417=VERTEX_POINT('',#12020);
#2418=VERTEX_POINT('',#12070);
#2419=VERTEX_POINT('',#12071);
#2420=VERTEX_POINT('',#12073);
#2421=VERTEX_POINT('',#12087);
#2422=VERTEX_POINT('',#12109);
#2423=VERTEX_POINT('',#12110);
#2424=VERTEX_POINT('',#12112);
#2425=VERTEX_POINT('',#12119);
#2426=VERTEX_POINT('',#12129);
#2427=VERTEX_POINT('',#12130);
#2428=VERTEX_POINT('',#12153);
#2429=VERTEX_POINT('',#12154);
#2430=VERTEX_POINT('',#12178);
#2431=VERTEX_POINT('',#12179);
#2432=VERTEX_POINT('',#12203);
#2433=VERTEX_POINT('',#12204);
#2434=VERTEX_POINT('',#12227);
#2435=VERTEX_POINT('',#12228);
#2436=VERTEX_POINT('',#12230);
#2437=VERTEX_POINT('',#12236);
#2438=VERTEX_POINT('',#12849);
#2439=VERTEX_POINT('',#12850);
#2440=VERTEX_POINT('',#12852);
#2441=VERTEX_POINT('',#12854);
#2442=VERTEX_POINT('',#12856);
#2443=VERTEX_POINT('',#12858);
#2444=VERTEX_POINT('',#12863);
#2445=VERTEX_POINT('',#12864);
#2446=VERTEX_POINT('',#12869);
#2447=VERTEX_POINT('',#12873);
#2448=VERTEX_POINT('',#12877);
#2449=VERTEX_POINT('',#12881);
#2450=VERTEX_POINT('',#12889);
#2451=VERTEX_POINT('',#12891);
#2452=EDGE_CURVE('',#2012,#2012,#1930,.T.);
#2453=EDGE_CURVE('',#2012,#2013,#1126,.T.);
#2454=EDGE_CURVE('',#2013,#2013,#1931,.T.);
#2455=EDGE_CURVE('',#2014,#2014,#1932,.T.);
#2456=EDGE_CURVE('',#2015,#2015,#1933,.T.);
#2457=EDGE_CURVE('',#2015,#2016,#1127,.T.);
#2458=EDGE_CURVE('',#2016,#2016,#1934,.T.);
#2459=EDGE_CURVE('',#2017,#2017,#1935,.T.);
#2460=EDGE_CURVE('',#2018,#2018,#1936,.T.);
#2461=EDGE_CURVE('',#2018,#2019,#1128,.T.);
#2462=EDGE_CURVE('',#2019,#2019,#1937,.T.);
#2463=EDGE_CURVE('',#2020,#2020,#1938,.T.);
#2464=EDGE_CURVE('',#2020,#2021,#1129,.T.);
#2465=EDGE_CURVE('',#2021,#2021,#1939,.T.);
#2466=EDGE_CURVE('',#2022,#2022,#1940,.T.);
#2467=EDGE_CURVE('',#2022,#2023,#1130,.T.);
#2468=EDGE_CURVE('',#2023,#2023,#1941,.T.);
#2469=EDGE_CURVE('',#2024,#2024,#1942,.T.);
#2470=EDGE_CURVE('',#2024,#2025,#1131,.T.);
#2471=EDGE_CURVE('',#2025,#2025,#1943,.T.);
#2472=EDGE_CURVE('',#2026,#2026,#1944,.T.);
#2473=EDGE_CURVE('',#2026,#2014,#1132,.T.);
#2474=EDGE_CURVE('',#2027,#2027,#1945,.T.);
#2475=EDGE_CURVE('',#2027,#2017,#1133,.T.);
#2476=EDGE_CURVE('',#2028,#2029,#1134,.T.);
#2477=EDGE_CURVE('',#2030,#2028,#1135,.T.);
#2478=EDGE_CURVE('',#2031,#2030,#1136,.T.);
#2479=EDGE_CURVE('',#2029,#2031,#1137,.T.);
#2480=EDGE_CURVE('',#2032,#2033,#1138,.T.);
#2481=EDGE_CURVE('',#2034,#2032,#1139,.T.);
#2482=EDGE_CURVE('',#2035,#2034,#1140,.T.);
#2483=EDGE_CURVE('',#2033,#2035,#1141,.T.);
#2484=EDGE_CURVE('',#2036,#2037,#1142,.T.);
#2485=EDGE_CURVE('',#2038,#2036,#1143,.T.);
#2486=EDGE_CURVE('',#2039,#2038,#1144,.T.);
#2487=EDGE_CURVE('',#2039,#2037,#1145,.T.);
#2488=EDGE_CURVE('',#2040,#2041,#1146,.T.);
#2489=EDGE_CURVE('',#2042,#2040,#1147,.T.);
#2490=EDGE_CURVE('',#2043,#2042,#1148,.T.);
#2491=EDGE_CURVE('',#2043,#2041,#1149,.T.);
#2492=EDGE_CURVE('',#2044,#2032,#1150,.T.);
#2493=EDGE_CURVE('',#2045,#2044,#1151,.T.);
#2494=EDGE_CURVE('',#2046,#2045,#1152,.T.);
#2495=EDGE_CURVE('',#2047,#2046,#1153,.T.);
#2496=EDGE_CURVE('',#2041,#2047,#1154,.T.);
#2497=EDGE_CURVE('',#2043,#2048,#1155,.T.);
#2498=EDGE_CURVE('',#2049,#2048,#1156,.T.);
#2499=EDGE_CURVE('',#2037,#2049,#1157,.T.);
#2500=EDGE_CURVE('',#2039,#2050,#1158,.T.);
#2501=EDGE_CURVE('',#2051,#2050,#1159,.T.);
#2502=EDGE_CURVE('',#2052,#2051,#1160,.T.);
#2503=EDGE_CURVE('',#2053,#2052,#1161,.T.);
#2504=EDGE_CURVE('',#2053,#2030,#1162,.T.);
#2505=EDGE_CURVE('',#2054,#2028,#1163,.T.);
#2506=EDGE_CURVE('',#2055,#2054,#1164,.T.);
#2507=EDGE_CURVE('',#2055,#2034,#1165,.T.);
#2508=EDGE_CURVE('',#2056,#2047,#1166,.T.);
#2509=EDGE_CURVE('',#2040,#2056,#1167,.T.);
#2510=EDGE_CURVE('',#2057,#2033,#1168,.T.);
#2511=EDGE_CURVE('',#2044,#2057,#1169,.T.);
#2512=EDGE_CURVE('',#2058,#2056,#1170,.T.);
#2513=EDGE_CURVE('',#2058,#2042,#1171,.T.);
#2514=EDGE_CURVE('',#2035,#2059,#1172,.T.);
#2515=EDGE_CURVE('',#2059,#2057,#1173,.T.);
#2516=EDGE_CURVE('',#2048,#2058,#1174,.T.);
#2517=EDGE_CURVE('',#2059,#2055,#1175,.T.);
#2518=EDGE_CURVE('',#2060,#2049,#1176,.T.);
#2519=EDGE_CURVE('',#2036,#2060,#1177,.T.);
#2520=EDGE_CURVE('',#2061,#2029,#1178,.T.);
#2521=EDGE_CURVE('',#2054,#2061,#1179,.T.);
#2522=EDGE_CURVE('',#2062,#2060,#1180,.T.);
#2523=EDGE_CURVE('',#2062,#2038,#1181,.T.);
#2524=EDGE_CURVE('',#2031,#2063,#1182,.T.);
#2525=EDGE_CURVE('',#2063,#2061,#1183,.T.);
#2526=EDGE_CURVE('',#2050,#2062,#1184,.T.);
#2527=EDGE_CURVE('',#2063,#2053,#1185,.T.);
#2528=EDGE_CURVE('',#2052,#2064,#1186,.T.);
#2529=EDGE_CURVE('',#2064,#2065,#1187,.T.);
#2530=EDGE_CURVE('',#2045,#2065,#1188,.T.);
#2531=EDGE_CURVE('',#2066,#2051,#1189,.T.);
#2532=EDGE_CURVE('',#2064,#2066,#1190,.T.);
#2533=EDGE_CURVE('',#2067,#2046,#1191,.T.);
#2534=EDGE_CURVE('',#2066,#2067,#1192,.T.);
#2535=EDGE_CURVE('',#2065,#2067,#1193,.T.);
#2536=EDGE_CURVE('',#2068,#2068,#1946,.T.);
#2537=EDGE_CURVE('',#2068,#2069,#1194,.T.);
#2538=EDGE_CURVE('',#2069,#2069,#1947,.T.);
#2539=EDGE_CURVE('',#2070,#2070,#1948,.T.);
#2540=EDGE_CURVE('',#2070,#2071,#1195,.T.);
#2541=EDGE_CURVE('',#2071,#2071,#1949,.T.);
#2542=EDGE_CURVE('',#2072,#2072,#1950,.T.);
#2543=EDGE_CURVE('',#2072,#2073,#1196,.T.);
#2544=EDGE_CURVE('',#2073,#2073,#1951,.T.);
#2545=EDGE_CURVE('',#2074,#2074,#1952,.T.);
#2546=EDGE_CURVE('',#2074,#2075,#1197,.T.);
#2547=EDGE_CURVE('',#2075,#2075,#1953,.T.);
#2548=EDGE_CURVE('',#2076,#2076,#1954,.T.);
#2549=EDGE_CURVE('',#2076,#2077,#1198,.T.);
#2550=EDGE_CURVE('',#2077,#2077,#1955,.T.);
#2551=EDGE_CURVE('',#2078,#2078,#1956,.T.);
#2552=EDGE_CURVE('',#2078,#2079,#1199,.T.);
#2553=EDGE_CURVE('',#2079,#2079,#1957,.T.);
#2554=EDGE_CURVE('',#2080,#2081,#1200,.T.);
#2555=EDGE_CURVE('',#2082,#2080,#1201,.T.);
#2556=EDGE_CURVE('',#2083,#2082,#1202,.T.);
#2557=EDGE_CURVE('',#2081,#2083,#1203,.T.);
#2558=EDGE_CURVE('',#2084,#2085,#1204,.T.);
#2559=EDGE_CURVE('',#2086,#2084,#1205,.T.);
#2560=EDGE_CURVE('',#2087,#2086,#1206,.T.);
#2561=EDGE_CURVE('',#2085,#2087,#1207,.T.);
#2562=EDGE_CURVE('',#2088,#2089,#1208,.T.);
#2563=EDGE_CURVE('',#2090,#2088,#1209,.T.);
#2564=EDGE_CURVE('',#2091,#2090,#1210,.T.);
#2565=EDGE_CURVE('',#2091,#2089,#1211,.T.);
#2566=EDGE_CURVE('',#2092,#2093,#1212,.T.);
#2567=EDGE_CURVE('',#2094,#2092,#1213,.T.);
#2568=EDGE_CURVE('',#2095,#2094,#1214,.T.);
#2569=EDGE_CURVE('',#2095,#2093,#1215,.T.);
#2570=EDGE_CURVE('',#2096,#2084,#1216,.T.);
#2571=EDGE_CURVE('',#2097,#2096,#1217,.T.);
#2572=EDGE_CURVE('',#2098,#2097,#1218,.T.);
#2573=EDGE_CURVE('',#2099,#2098,#1219,.T.);
#2574=EDGE_CURVE('',#2093,#2099,#1220,.T.);
#2575=EDGE_CURVE('',#2095,#2100,#1221,.T.);
#2576=EDGE_CURVE('',#2101,#2100,#1222,.T.);
#2577=EDGE_CURVE('',#2089,#2101,#1223,.T.);
#2578=EDGE_CURVE('',#2091,#2102,#1224,.T.);
#2579=EDGE_CURVE('',#2103,#2102,#1225,.T.);
#2580=EDGE_CURVE('',#2104,#2103,#1226,.T.);
#2581=EDGE_CURVE('',#2105,#2104,#1227,.T.);
#2582=EDGE_CURVE('',#2105,#2082,#1228,.T.);
#2583=EDGE_CURVE('',#2106,#2080,#1229,.T.);
#2584=EDGE_CURVE('',#2107,#2106,#1230,.T.);
#2585=EDGE_CURVE('',#2107,#2086,#1231,.T.);
#2586=EDGE_CURVE('',#2108,#2099,#1232,.T.);
#2587=EDGE_CURVE('',#2092,#2108,#1233,.T.);
#2588=EDGE_CURVE('',#2109,#2085,#1234,.T.);
#2589=EDGE_CURVE('',#2096,#2109,#1235,.T.);
#2590=EDGE_CURVE('',#2110,#2108,#1236,.T.);
#2591=EDGE_CURVE('',#2110,#2094,#1237,.T.);
#2592=EDGE_CURVE('',#2087,#2111,#1238,.T.);
#2593=EDGE_CURVE('',#2111,#2109,#1239,.T.);
#2594=EDGE_CURVE('',#2100,#2110,#1240,.T.);
#2595=EDGE_CURVE('',#2111,#2107,#1241,.T.);
#2596=EDGE_CURVE('',#2112,#2101,#1242,.T.);
#2597=EDGE_CURVE('',#2088,#2112,#1243,.T.);
#2598=EDGE_CURVE('',#2113,#2081,#1244,.T.);
#2599=EDGE_CURVE('',#2106,#2113,#1245,.T.);
#2600=EDGE_CURVE('',#2114,#2112,#1246,.T.);
#2601=EDGE_CURVE('',#2114,#2090,#1247,.T.);
#2602=EDGE_CURVE('',#2083,#2115,#1248,.T.);
#2603=EDGE_CURVE('',#2115,#2113,#1249,.T.);
#2604=EDGE_CURVE('',#2102,#2114,#1250,.T.);
#2605=EDGE_CURVE('',#2115,#2105,#1251,.T.);
#2606=EDGE_CURVE('',#2104,#2116,#1252,.T.);
#2607=EDGE_CURVE('',#2116,#2117,#1253,.T.);
#2608=EDGE_CURVE('',#2097,#2117,#1254,.T.);
#2609=EDGE_CURVE('',#2118,#2103,#1255,.T.);
#2610=EDGE_CURVE('',#2116,#2118,#1256,.T.);
#2611=EDGE_CURVE('',#2119,#2098,#1257,.T.);
#2612=EDGE_CURVE('',#2118,#2119,#1258,.T.);
#2613=EDGE_CURVE('',#2117,#2119,#1259,.T.);
#2614=EDGE_CURVE('',#2120,#2121,#1260,.T.);
#2615=EDGE_CURVE('',#2122,#2120,#1261,.T.);
#2616=EDGE_CURVE('',#2123,#2122,#1262,.T.);
#2617=EDGE_CURVE('',#2121,#2123,#1263,.T.);
#2618=EDGE_CURVE('',#2124,#2125,#1264,.T.);
#2619=EDGE_CURVE('',#2126,#2124,#1265,.T.);
#2620=EDGE_CURVE('',#2127,#2126,#1266,.T.);
#2621=EDGE_CURVE('',#2125,#2127,#1267,.T.);
#2622=EDGE_CURVE('',#2123,#2126,#1268,.T.);
#2623=EDGE_CURVE('',#2127,#2122,#1269,.T.);
#2624=EDGE_CURVE('',#2128,#2120,#1270,.T.);
#2625=EDGE_CURVE('',#2129,#2128,#1271,.T.);
#2626=EDGE_CURVE('',#2129,#2130,#1272,.T.);
#2627=EDGE_CURVE('',#2130,#2131,#1273,.T.);
#2628=EDGE_CURVE('',#2125,#2131,#1274,.T.);
#2629=EDGE_CURVE('',#2121,#2132,#1275,.T.);
#2630=EDGE_CURVE('',#2132,#2128,#1276,.T.);
#2631=EDGE_CURVE('',#2130,#2133,#1277,.T.);
#2632=EDGE_CURVE('',#2133,#2134,#1278,.T.);
#2633=EDGE_CURVE('',#2131,#2134,#1279,.T.);
#2634=EDGE_CURVE('',#2135,#2129,#1280,.T.);
#2635=EDGE_CURVE('',#2135,#2132,#1281,.T.);
#2636=EDGE_CURVE('',#2134,#2124,#1282,.T.);
#2637=EDGE_CURVE('',#2133,#2135,#1283,.T.);
#2638=EDGE_CURVE('',#2136,#2137,#1284,.T.);
#2639=EDGE_CURVE('',#2137,#2138,#1285,.T.);
#2640=EDGE_CURVE('',#2139,#2138,#1286,.T.);
#2641=EDGE_CURVE('',#2136,#2139,#1287,.T.);
#2642=EDGE_CURVE('',#2140,#2136,#1288,.T.);
#2643=EDGE_CURVE('',#2141,#2139,#1289,.T.);
#2644=EDGE_CURVE('',#2140,#2141,#1290,.T.);
#2645=EDGE_CURVE('',#2142,#2140,#1291,.T.);
#2646=EDGE_CURVE('',#2143,#2141,#1292,.T.);
#2647=EDGE_CURVE('',#2142,#2143,#1293,.T.);
#2648=EDGE_CURVE('',#2137,#2142,#1294,.T.);
#2649=EDGE_CURVE('',#2138,#2143,#1295,.T.);
#2650=EDGE_CURVE('',#2144,#2145,#1296,.T.);
#2651=EDGE_CURVE('',#2144,#2146,#1297,.T.);
#2652=EDGE_CURVE('',#2147,#2146,#1298,.T.);
#2653=EDGE_CURVE('',#2145,#2147,#1299,.T.);
#2654=EDGE_CURVE('',#2148,#2144,#1300,.T.);
#2655=EDGE_CURVE('',#2149,#2148,#1301,.T.);
#2656=EDGE_CURVE('',#2146,#2149,#1302,.T.);
#2657=EDGE_CURVE('',#2150,#2147,#1303,.T.);
#2658=EDGE_CURVE('',#2151,#2150,#1304,.T.);
#2659=EDGE_CURVE('',#2151,#2145,#1305,.T.);
#2660=EDGE_CURVE('',#2148,#2152,#1306,.T.);
#2661=EDGE_CURVE('',#2152,#2153,#1307,.T.);
#2662=EDGE_CURVE('',#2149,#2153,#1308,.T.);
#2663=EDGE_CURVE('',#2154,#2151,#1309,.T.);
#2664=EDGE_CURVE('',#2155,#2150,#1310,.T.);
#2665=EDGE_CURVE('',#2154,#2155,#1311,.T.);
#2666=EDGE_CURVE('',#2152,#2154,#1312,.T.);
#2667=EDGE_CURVE('',#2153,#2155,#1313,.T.);
#2668=EDGE_CURVE('',#2156,#2157,#1314,.T.);
#2669=EDGE_CURVE('',#2156,#2158,#1315,.T.);
#2670=EDGE_CURVE('',#2159,#2158,#1316,.T.);
#2671=EDGE_CURVE('',#2157,#2159,#1317,.T.);
#2672=EDGE_CURVE('',#2160,#2156,#1958,.T.);
#2673=EDGE_CURVE('',#2160,#2161,#1318,.T.);
#2674=EDGE_CURVE('',#2158,#2161,#1959,.T.);
#2675=EDGE_CURVE('',#2162,#2160,#1319,.T.);
#2676=EDGE_CURVE('',#2162,#2163,#1320,.T.);
#2677=EDGE_CURVE('',#2161,#2163,#1321,.T.);
#2678=EDGE_CURVE('',#2157,#2162,#1960,.T.);
#2679=EDGE_CURVE('',#2163,#2159,#1961,.T.);
#2680=EDGE_CURVE('',#2164,#2164,#1962,.T.);
#2681=EDGE_CURVE('',#2164,#2165,#1322,.T.);
#2682=EDGE_CURVE('',#2165,#2165,#1963,.T.);
#2683=EDGE_CURVE('',#2166,#2166,#1964,.T.);
#2684=EDGE_CURVE('',#2166,#2167,#1323,.T.);
#2685=EDGE_CURVE('',#2167,#2167,#1965,.T.);
#2686=EDGE_CURVE('',#2168,#2169,#1324,.T.);
#2687=EDGE_CURVE('',#2169,#2170,#1325,.T.);
#2688=EDGE_CURVE('',#2171,#2170,#1326,.T.);
#2689=EDGE_CURVE('',#2168,#2171,#1327,.T.);
#2690=EDGE_CURVE('',#2172,#2168,#1328,.T.);
#2691=EDGE_CURVE('',#2173,#2171,#1329,.T.);
#2692=EDGE_CURVE('',#2172,#2173,#1330,.T.);
#2693=EDGE_CURVE('',#2174,#2172,#1331,.T.);
#2694=EDGE_CURVE('',#2175,#2173,#1332,.T.);
#2695=EDGE_CURVE('',#2174,#2175,#1333,.T.);
#2696=EDGE_CURVE('',#2169,#2174,#1334,.T.);
#2697=EDGE_CURVE('',#2170,#2175,#1335,.T.);
#2698=EDGE_CURVE('',#2176,#2176,#1966,.T.);
#2699=EDGE_CURVE('',#2176,#2177,#1336,.T.);
#2700=EDGE_CURVE('',#2177,#2177,#1967,.T.);
#2701=EDGE_CURVE('',#2178,#2178,#1968,.T.);
#2702=EDGE_CURVE('',#2178,#2179,#1337,.T.);
#2703=EDGE_CURVE('',#2179,#2179,#1969,.T.);
#2704=EDGE_CURVE('',#2180,#2181,#1338,.T.);
#2705=EDGE_CURVE('',#2182,#2180,#1970,.T.);
#2706=EDGE_CURVE('',#2183,#2182,#1339,.T.);
#2707=EDGE_CURVE('',#2181,#2183,#1340,.T.);
#2708=EDGE_CURVE('',#2184,#2180,#1341,.T.);
#2709=EDGE_CURVE('',#2185,#2184,#1971,.T.);
#2710=EDGE_CURVE('',#2182,#2185,#1342,.T.);
#2711=EDGE_CURVE('',#2186,#2184,#1343,.T.);
#2712=EDGE_CURVE('',#2187,#2186,#1344,.T.);
#2713=EDGE_CURVE('',#2185,#2187,#1345,.T.);
#2714=EDGE_CURVE('',#2188,#2187,#1346,.T.);
#2715=EDGE_CURVE('',#2188,#2189,#1347,.T.);
#2716=EDGE_CURVE('',#2189,#2190,#1348,.T.);
#2717=EDGE_CURVE('',#2190,#2191,#1349,.T.);
#2718=EDGE_CURVE('',#2191,#2192,#1350,.T.);
#2719=EDGE_CURVE('',#2193,#2192,#1351,.T.);
#2720=EDGE_CURVE('',#2193,#2194,#1352,.T.);
#2721=EDGE_CURVE('',#2194,#2195,#1353,.T.);
#2722=EDGE_CURVE('',#2183,#2195,#1354,.T.);
#2723=EDGE_CURVE('',#2196,#2186,#1355,.T.);
#2724=EDGE_CURVE('',#2196,#2197,#1356,.T.);
#2725=EDGE_CURVE('',#2197,#2198,#1357,.T.);
#2726=EDGE_CURVE('',#2198,#2188,#1358,.T.);
#2727=EDGE_CURVE('',#2195,#2199,#1359,.T.);
#2728=EDGE_CURVE('',#2199,#2200,#1360,.T.);
#2729=EDGE_CURVE('',#2201,#2200,#1361,.T.);
#2730=EDGE_CURVE('',#2181,#2201,#1362,.T.);
#2731=EDGE_CURVE('',#2202,#2194,#1972,.T.);
#2732=EDGE_CURVE('',#2203,#2202,#1363,.T.);
#2733=EDGE_CURVE('',#2199,#2203,#1973,.T.);
#2734=EDGE_CURVE('',#2204,#2193,#1974,.T.);
#2735=EDGE_CURVE('',#2202,#2204,#1364,.T.);
#2736=EDGE_CURVE('',#2205,#2203,#1365,.T.);
#2737=EDGE_CURVE('',#2200,#2205,#1975,.T.);
#2738=EDGE_CURVE('',#2192,#2206,#1366,.T.);
#2739=EDGE_CURVE('',#2206,#2204,#1367,.T.);
#2740=EDGE_CURVE('',#2205,#2201,#1368,.T.);
#2741=EDGE_CURVE('',#2207,#2206,#1369,.T.);
#2742=EDGE_CURVE('',#2207,#2208,#1370,.T.);
#2743=EDGE_CURVE('',#2208,#2209,#1371,.T.);
#2744=EDGE_CURVE('',#2209,#2210,#1372,.T.);
#2745=EDGE_CURVE('',#2210,#2211,#1373,.T.);
#2746=EDGE_CURVE('',#2211,#2196,#1374,.T.);
#2747=EDGE_CURVE('',#2197,#2211,#1976,.T.);
#2748=EDGE_CURVE('',#2198,#2210,#1977,.T.);
#2749=EDGE_CURVE('',#2209,#2189,#1978,.T.);
#2750=EDGE_CURVE('',#2208,#2190,#1979,.T.);
#2751=EDGE_CURVE('',#2191,#2207,#1375,.T.);
#2752=EDGE_CURVE('',#2212,#2212,#1980,.T.);
#2753=EDGE_CURVE('',#2212,#2213,#1376,.T.);
#2754=EDGE_CURVE('',#2213,#2213,#1981,.T.);
#2755=EDGE_CURVE('',#2214,#2214,#1982,.T.);
#2756=EDGE_CURVE('',#2214,#2215,#1377,.T.);
#2757=EDGE_CURVE('',#2215,#2215,#1983,.T.);
#2758=EDGE_CURVE('',#2216,#2217,#1378,.T.);
#2759=EDGE_CURVE('',#2216,#2218,#1984,.T.);
#2760=EDGE_CURVE('',#2217,#2218,#1379,.T.);
#2761=EDGE_CURVE('',#2219,#2216,#1380,.T.);
#2762=EDGE_CURVE('',#2220,#2219,#1985,.T.);
#2763=EDGE_CURVE('',#2218,#2220,#1381,.T.);
#2764=EDGE_CURVE('',#2221,#2217,#1382,.T.);
#2765=EDGE_CURVE('',#2221,#2222,#1383,.T.);
#2766=EDGE_CURVE('',#2222,#2223,#1384,.T.);
#2767=EDGE_CURVE('',#2223,#2224,#1385,.T.);
#2768=EDGE_CURVE('',#2225,#2224,#1386,.T.);
#2769=EDGE_CURVE('',#2225,#2226,#1387,.T.);
#2770=EDGE_CURVE('',#2226,#2227,#1388,.T.);
#2771=EDGE_CURVE('',#2227,#2228,#1389,.T.);
#2772=EDGE_CURVE('',#2228,#2229,#1390,.T.);
#2773=EDGE_CURVE('',#2219,#2229,#1391,.T.);
#2774=EDGE_CURVE('',#2230,#2220,#1392,.T.);
#2775=EDGE_CURVE('',#2231,#2230,#1393,.T.);
#2776=EDGE_CURVE('',#2231,#2232,#1394,.T.);
#2777=EDGE_CURVE('',#2232,#2233,#1395,.T.);
#2778=EDGE_CURVE('',#2233,#2225,#1396,.T.);
#2779=EDGE_CURVE('',#2224,#2234,#1397,.T.);
#2780=EDGE_CURVE('',#2234,#2235,#1398,.T.);
#2781=EDGE_CURVE('',#2235,#2221,#1399,.T.);
#2782=EDGE_CURVE('',#2226,#2233,#1986,.T.);
#2783=EDGE_CURVE('',#2227,#2232,#1987,.T.);
#2784=EDGE_CURVE('',#2236,#2231,#1400,.T.);
#2785=EDGE_CURVE('',#2228,#2236,#1401,.T.);
#2786=EDGE_CURVE('',#2235,#2222,#1988,.T.);
#2787=EDGE_CURVE('',#2237,#2237,#1989,.T.);
#2788=EDGE_CURVE('',#2237,#2238,#1402,.T.);
#2789=EDGE_CURVE('',#2238,#2238,#1990,.T.);
#2790=EDGE_CURVE('',#2234,#2223,#1991,.T.);
#2791=EDGE_CURVE('',#2239,#2230,#1403,.T.);
#2792=EDGE_CURVE('',#2236,#2239,#1404,.T.);
#2793=EDGE_CURVE('',#2229,#2239,#1405,.T.);
#2794=EDGE_CURVE('',#2240,#2240,#1992,.T.);
#2795=EDGE_CURVE('',#2241,#2241,#1993,.T.);
#2796=EDGE_CURVE('',#2242,#2242,#1994,.T.);
#2797=EDGE_CURVE('',#2242,#2240,#1406,.T.);
#2798=EDGE_CURVE('',#2243,#2243,#1995,.T.);
#2799=EDGE_CURVE('',#2244,#2244,#1996,.T.);
#2800=EDGE_CURVE('',#2243,#2245,#1407,.T.);
#2801=EDGE_CURVE('',#2245,#2245,#1997,.T.);
#2802=EDGE_CURVE('',#2241,#2244,#1408,.T.);
#2803=EDGE_CURVE('',#2246,#2247,#1409,.T.);
#2804=EDGE_CURVE('',#2246,#2248,#175,.T.);
#2805=EDGE_CURVE('',#2248,#2249,#1998,.F.);
#2806=EDGE_CURVE('',#2249,#2247,#176,.T.);
#2807=EDGE_CURVE('',#2250,#2251,#1410,.T.);
#2808=EDGE_CURVE('',#2250,#2246,#177,.T.);
#2809=EDGE_CURVE('',#2247,#2251,#178,.T.);
#2810=EDGE_CURVE('',#2252,#2253,#1411,.T.);
#2811=EDGE_CURVE('',#2252,#2250,#179,.T.);
#2812=EDGE_CURVE('',#2251,#2253,#180,.T.);
#2813=EDGE_CURVE('',#2254,#2255,#1412,.T.);
#2814=EDGE_CURVE('',#2254,#2252,#181,.T.);
#2815=EDGE_CURVE('',#2253,#2255,#182,.T.);
#2816=EDGE_CURVE('',#2256,#2257,#1413,.T.);
#2817=EDGE_CURVE('',#2256,#2254,#183,.T.);
#2818=EDGE_CURVE('',#2255,#2257,#184,.T.);
#2819=EDGE_CURVE('',#2258,#2259,#1414,.T.);
#2820=EDGE_CURVE('',#2258,#2256,#185,.T.);
#2821=EDGE_CURVE('',#2257,#2259,#186,.T.);
#2822=EDGE_CURVE('',#2260,#2261,#1415,.T.);
#2823=EDGE_CURVE('',#2260,#2258,#187,.T.);
#2824=EDGE_CURVE('',#2259,#2261,#188,.T.);
#2825=EDGE_CURVE('',#2262,#2263,#1416,.T.);
#2826=EDGE_CURVE('',#2262,#2260,#189,.T.);
#2827=EDGE_CURVE('',#2261,#2263,#190,.T.);
#2828=EDGE_CURVE('',#2264,#2265,#1417,.T.);
#2829=EDGE_CURVE('',#2264,#2262,#191,.T.);
#2830=EDGE_CURVE('',#2263,#2265,#192,.T.);
#2831=EDGE_CURVE('',#2266,#2267,#1418,.T.);
#2832=EDGE_CURVE('',#2266,#2264,#193,.T.);
#2833=EDGE_CURVE('',#2265,#2267,#194,.T.);
#2834=EDGE_CURVE('',#2268,#2269,#1419,.T.);
#2835=EDGE_CURVE('',#2268,#2266,#195,.T.);
#2836=EDGE_CURVE('',#2267,#2269,#196,.T.);
#2837=EDGE_CURVE('',#2270,#2271,#1420,.T.);
#2838=EDGE_CURVE('',#2270,#2268,#197,.T.);
#2839=EDGE_CURVE('',#2269,#2271,#198,.T.);
#2840=EDGE_CURVE('',#2272,#2273,#1421,.T.);
#2841=EDGE_CURVE('',#2272,#2270,#199,.T.);
#2842=EDGE_CURVE('',#2271,#2273,#200,.T.);
#2843=EDGE_CURVE('',#2274,#2275,#1422,.T.);
#2844=EDGE_CURVE('',#2274,#2272,#201,.T.);
#2845=EDGE_CURVE('',#2273,#2275,#202,.T.);
#2846=EDGE_CURVE('',#2276,#2277,#1423,.T.);
#2847=EDGE_CURVE('',#2276,#2274,#203,.T.);
#2848=EDGE_CURVE('',#2275,#2277,#204,.T.);
#2849=EDGE_CURVE('',#2278,#2279,#1424,.T.);
#2850=EDGE_CURVE('',#2278,#2276,#205,.T.);
#2851=EDGE_CURVE('',#2277,#2279,#206,.T.);
#2852=EDGE_CURVE('',#2280,#2281,#1425,.T.);
#2853=EDGE_CURVE('',#2280,#2278,#207,.T.);
#2854=EDGE_CURVE('',#2279,#2281,#208,.T.);
#2855=EDGE_CURVE('',#2282,#2283,#1426,.T.);
#2856=EDGE_CURVE('',#2282,#2280,#209,.T.);
#2857=EDGE_CURVE('',#2281,#2283,#210,.T.);
#2858=EDGE_CURVE('',#2284,#2285,#1427,.T.);
#2859=EDGE_CURVE('',#2284,#2282,#211,.T.);
#2860=EDGE_CURVE('',#2283,#2285,#212,.T.);
#2861=EDGE_CURVE('',#2286,#2287,#1428,.T.);
#2862=EDGE_CURVE('',#2286,#2284,#213,.T.);
#2863=EDGE_CURVE('',#2285,#2287,#214,.T.);
#2864=EDGE_CURVE('',#2288,#2289,#1429,.T.);
#2865=EDGE_CURVE('',#2288,#2286,#215,.T.);
#2866=EDGE_CURVE('',#2287,#2289,#216,.T.);
#2867=EDGE_CURVE('',#2290,#2291,#1430,.T.);
#2868=EDGE_CURVE('',#2290,#2288,#217,.T.);
#2869=EDGE_CURVE('',#2289,#2291,#218,.T.);
#2870=EDGE_CURVE('',#2292,#2293,#1431,.T.);
#2871=EDGE_CURVE('',#2292,#2290,#219,.T.);
#2872=EDGE_CURVE('',#2291,#2293,#220,.T.);
#2873=EDGE_CURVE('',#2294,#2295,#1432,.T.);
#2874=EDGE_CURVE('',#2294,#2292,#221,.T.);
#2875=EDGE_CURVE('',#2293,#2295,#222,.T.);
#2876=EDGE_CURVE('',#2296,#2297,#1433,.T.);
#2877=EDGE_CURVE('',#2296,#2294,#223,.T.);
#2878=EDGE_CURVE('',#2295,#2297,#224,.T.);
#2879=EDGE_CURVE('',#2298,#2299,#1434,.T.);
#2880=EDGE_CURVE('',#2298,#2296,#225,.T.);
#2881=EDGE_CURVE('',#2297,#2299,#226,.T.);
#2882=EDGE_CURVE('',#2300,#2301,#1435,.T.);
#2883=EDGE_CURVE('',#2300,#2298,#227,.T.);
#2884=EDGE_CURVE('',#2299,#2301,#228,.T.);
#2885=EDGE_CURVE('',#2302,#2303,#1436,.T.);
#2886=EDGE_CURVE('',#2302,#2300,#229,.T.);
#2887=EDGE_CURVE('',#2301,#2303,#230,.T.);
#2888=EDGE_CURVE('',#2304,#2305,#1437,.T.);
#2889=EDGE_CURVE('',#2304,#2302,#231,.T.);
#2890=EDGE_CURVE('',#2303,#2305,#232,.T.);
#2891=EDGE_CURVE('',#2306,#2307,#1438,.T.);
#2892=EDGE_CURVE('',#2306,#2304,#233,.T.);
#2893=EDGE_CURVE('',#2305,#2307,#234,.T.);
#2894=EDGE_CURVE('',#2308,#2309,#1439,.T.);
#2895=EDGE_CURVE('',#2308,#2306,#235,.T.);
#2896=EDGE_CURVE('',#2307,#2309,#236,.T.);
#2897=EDGE_CURVE('',#2310,#2311,#1440,.T.);
#2898=EDGE_CURVE('',#2310,#2308,#237,.T.);
#2899=EDGE_CURVE('',#2309,#2311,#238,.T.);
#2900=EDGE_CURVE('',#2312,#2313,#1441,.T.);
#2901=EDGE_CURVE('',#2312,#2310,#239,.T.);
#2902=EDGE_CURVE('',#2311,#2313,#240,.T.);
#2903=EDGE_CURVE('',#2314,#2315,#1442,.T.);
#2904=EDGE_CURVE('',#2314,#2312,#241,.T.);
#2905=EDGE_CURVE('',#2313,#2315,#242,.T.);
#2906=EDGE_CURVE('',#2316,#2317,#1443,.T.);
#2907=EDGE_CURVE('',#2318,#2316,#1999,.F.);
#2908=EDGE_CURVE('',#2318,#2314,#243,.T.);
#2909=EDGE_CURVE('',#2315,#2317,#244,.T.);
#2910=EDGE_CURVE('',#2319,#2320,#1444,.T.);
#2911=EDGE_CURVE('',#2319,#2321,#245,.T.);
#2912=EDGE_CURVE('',#2322,#2321,#2000,.T.);
#2913=EDGE_CURVE('',#2320,#2322,#246,.T.);
#2914=EDGE_CURVE('',#2323,#2324,#1445,.T.);
#2915=EDGE_CURVE('',#2323,#2319,#247,.T.);
#2916=EDGE_CURVE('',#2324,#2320,#248,.T.);
#2917=EDGE_CURVE('',#2325,#2326,#1446,.T.);
#2918=EDGE_CURVE('',#2325,#2323,#249,.T.);
#2919=EDGE_CURVE('',#2326,#2324,#250,.T.);
#2920=EDGE_CURVE('',#2327,#2328,#1447,.T.);
#2921=EDGE_CURVE('',#2327,#2325,#251,.T.);
#2922=EDGE_CURVE('',#2328,#2326,#252,.T.);
#2923=EDGE_CURVE('',#2329,#2330,#1448,.T.);
#2924=EDGE_CURVE('',#2329,#2327,#253,.T.);
#2925=EDGE_CURVE('',#2330,#2328,#254,.T.);
#2926=EDGE_CURVE('',#2331,#2332,#1449,.T.);
#2927=EDGE_CURVE('',#2331,#2329,#255,.T.);
#2928=EDGE_CURVE('',#2332,#2330,#256,.T.);
#2929=EDGE_CURVE('',#2333,#2334,#1450,.T.);
#2930=EDGE_CURVE('',#2333,#2331,#257,.T.);
#2931=EDGE_CURVE('',#2334,#2332,#258,.T.);
#2932=EDGE_CURVE('',#2335,#2336,#1451,.T.);
#2933=EDGE_CURVE('',#2335,#2333,#259,.T.);
#2934=EDGE_CURVE('',#2336,#2334,#260,.T.);
#2935=EDGE_CURVE('',#2337,#2338,#1452,.T.);
#2936=EDGE_CURVE('',#2337,#2335,#261,.T.);
#2937=EDGE_CURVE('',#2338,#2336,#262,.T.);
#2938=EDGE_CURVE('',#2339,#2340,#1453,.T.);
#2939=EDGE_CURVE('',#2339,#2337,#263,.T.);
#2940=EDGE_CURVE('',#2340,#2338,#264,.T.);
#2941=EDGE_CURVE('',#2341,#2342,#1454,.T.);
#2942=EDGE_CURVE('',#2341,#2339,#265,.T.);
#2943=EDGE_CURVE('',#2342,#2340,#266,.T.);
#2944=EDGE_CURVE('',#2343,#2344,#1455,.T.);
#2945=EDGE_CURVE('',#2343,#2341,#267,.T.);
#2946=EDGE_CURVE('',#2344,#2342,#268,.T.);
#2947=EDGE_CURVE('',#2345,#2346,#1456,.T.);
#2948=EDGE_CURVE('',#2345,#2343,#269,.T.);
#2949=EDGE_CURVE('',#2346,#2344,#270,.T.);
#2950=EDGE_CURVE('',#2347,#2348,#1457,.T.);
#2951=EDGE_CURVE('',#2347,#2345,#271,.T.);
#2952=EDGE_CURVE('',#2348,#2346,#272,.T.);
#2953=EDGE_CURVE('',#2349,#2350,#1458,.T.);
#2954=EDGE_CURVE('',#2349,#2347,#273,.T.);
#2955=EDGE_CURVE('',#2350,#2348,#274,.T.);
#2956=EDGE_CURVE('',#2351,#2352,#1459,.T.);
#2957=EDGE_CURVE('',#2351,#2349,#275,.T.);
#2958=EDGE_CURVE('',#2352,#2350,#276,.T.);
#2959=EDGE_CURVE('',#2353,#2354,#1460,.T.);
#2960=EDGE_CURVE('',#2353,#2351,#277,.T.);
#2961=EDGE_CURVE('',#2354,#2352,#278,.T.);
#2962=EDGE_CURVE('',#2355,#2356,#1461,.T.);
#2963=EDGE_CURVE('',#2355,#2353,#279,.T.);
#2964=EDGE_CURVE('',#2356,#2354,#280,.T.);
#2965=EDGE_CURVE('',#2357,#2358,#1462,.T.);
#2966=EDGE_CURVE('',#2357,#2355,#281,.T.);
#2967=EDGE_CURVE('',#2358,#2356,#282,.T.);
#2968=EDGE_CURVE('',#2359,#2360,#1463,.T.);
#2969=EDGE_CURVE('',#2359,#2357,#283,.T.);
#2970=EDGE_CURVE('',#2360,#2358,#284,.T.);
#2971=EDGE_CURVE('',#2361,#2362,#1464,.T.);
#2972=EDGE_CURVE('',#2361,#2359,#285,.T.);
#2973=EDGE_CURVE('',#2362,#2360,#286,.T.);
#2974=EDGE_CURVE('',#2363,#2364,#1465,.T.);
#2975=EDGE_CURVE('',#2363,#2361,#287,.T.);
#2976=EDGE_CURVE('',#2364,#2362,#288,.T.);
#2977=EDGE_CURVE('',#2365,#2366,#1466,.T.);
#2978=EDGE_CURVE('',#2365,#2363,#289,.T.);
#2979=EDGE_CURVE('',#2366,#2364,#290,.T.);
#2980=EDGE_CURVE('',#2367,#2368,#1467,.T.);
#2981=EDGE_CURVE('',#2367,#2365,#291,.T.);
#2982=EDGE_CURVE('',#2368,#2366,#292,.T.);
#2983=EDGE_CURVE('',#2369,#2370,#1468,.T.);
#2984=EDGE_CURVE('',#2369,#2367,#293,.T.);
#2985=EDGE_CURVE('',#2370,#2368,#294,.T.);
#2986=EDGE_CURVE('',#2371,#2372,#1469,.T.);
#2987=EDGE_CURVE('',#2371,#2369,#295,.T.);
#2988=EDGE_CURVE('',#2372,#2370,#296,.T.);
#2989=EDGE_CURVE('',#2373,#2374,#1470,.T.);
#2990=EDGE_CURVE('',#2373,#2371,#297,.T.);
#2991=EDGE_CURVE('',#2374,#2372,#298,.T.);
#2992=EDGE_CURVE('',#2375,#2376,#1471,.T.);
#2993=EDGE_CURVE('',#2375,#2373,#299,.T.);
#2994=EDGE_CURVE('',#2376,#2374,#300,.T.);
#2995=EDGE_CURVE('',#2377,#2378,#1472,.T.);
#2996=EDGE_CURVE('',#2377,#2375,#301,.T.);
#2997=EDGE_CURVE('',#2378,#2376,#302,.T.);
#2998=EDGE_CURVE('',#2379,#2380,#1473,.T.);
#2999=EDGE_CURVE('',#2379,#2377,#303,.T.);
#3000=EDGE_CURVE('',#2380,#2378,#304,.T.);
#3001=EDGE_CURVE('',#2381,#2382,#1474,.T.);
#3002=EDGE_CURVE('',#2381,#2379,#305,.T.);
#3003=EDGE_CURVE('',#2382,#2380,#306,.T.);
#3004=EDGE_CURVE('',#2383,#2384,#1475,.T.);
#3005=EDGE_CURVE('',#2383,#2381,#307,.T.);
#3006=EDGE_CURVE('',#2384,#2382,#308,.T.);
#3007=EDGE_CURVE('',#2385,#2386,#1476,.T.);
#3008=EDGE_CURVE('',#2385,#2383,#309,.T.);
#3009=EDGE_CURVE('',#2386,#2384,#310,.T.);
#3010=EDGE_CURVE('',#2387,#2388,#1477,.T.);
#3011=EDGE_CURVE('',#2387,#2385,#311,.T.);
#3012=EDGE_CURVE('',#2388,#2386,#312,.T.);
#3013=EDGE_CURVE('',#2389,#2322,#313,.T.);
#3014=EDGE_CURVE('',#2317,#2389,#314,.T.);
#3015=EDGE_CURVE('',#2390,#2249,#315,.T.);
#3016=EDGE_CURVE('',#2390,#2388,#316,.T.);
#3017=EDGE_CURVE('',#2391,#2390,#2001,.T.);
#3018=EDGE_CURVE('',#2391,#2387,#317,.T.);
#3019=EDGE_CURVE('',#2321,#2318,#318,.T.);
#3020=EDGE_CURVE('',#2248,#2391,#319,.T.);
#3021=EDGE_CURVE('',#2316,#2389,#2002,.F.);
#3022=EDGE_CURVE('',#2392,#2393,#1478,.T.);
#3023=EDGE_CURVE('',#2392,#2394,#1479,.T.);
#3024=EDGE_CURVE('',#2394,#2395,#1480,.T.);
#3025=EDGE_CURVE('',#2393,#2395,#1481,.T.);
#3026=EDGE_CURVE('',#2396,#2392,#1482,.T.);
#3027=EDGE_CURVE('',#2396,#2397,#1483,.T.);
#3028=EDGE_CURVE('',#2397,#2394,#1484,.T.);
#3029=EDGE_CURVE('',#2398,#2396,#1485,.T.);
#3030=EDGE_CURVE('',#2398,#2399,#1486,.T.);
#3031=EDGE_CURVE('',#2399,#2397,#1487,.T.);
#3032=EDGE_CURVE('',#2400,#2398,#1488,.T.);
#3033=EDGE_CURVE('',#2400,#2401,#1489,.T.);
#3034=EDGE_CURVE('',#2401,#2399,#1490,.T.);
#3035=EDGE_CURVE('',#2402,#2400,#1491,.T.);
#3036=EDGE_CURVE('',#2402,#2403,#1492,.T.);
#3037=EDGE_CURVE('',#2403,#2401,#1493,.T.);
#3038=EDGE_CURVE('',#2393,#2402,#1494,.T.);
#3039=EDGE_CURVE('',#2395,#2403,#1495,.T.);
#3040=EDGE_CURVE('',#2404,#2404,#2003,.T.);
#3041=EDGE_CURVE('',#2404,#2405,#1496,.T.);
#3042=EDGE_CURVE('',#2405,#2405,#2004,.T.);
#3043=EDGE_CURVE('',#2406,#2407,#1497,.T.);
#3044=EDGE_CURVE('',#2408,#2407,#2005,.F.);
#3045=EDGE_CURVE('',#2408,#2406,#320,.T.);
#3046=EDGE_CURVE('',#2409,#2410,#1498,.T.);
#3047=EDGE_CURVE('',#2410,#2411,#321,.T.);
#3048=EDGE_CURVE('',#2407,#2411,#2006,.F.);
#3049=EDGE_CURVE('',#2406,#2409,#322,.T.);
#3050=EDGE_CURVE('',#2412,#2413,#1499,.T.);
#3051=EDGE_CURVE('',#2413,#2410,#323,.T.);
#3052=EDGE_CURVE('',#2409,#2412,#324,.T.);
#3053=EDGE_CURVE('',#2414,#2415,#1500,.T.);
#3054=EDGE_CURVE('',#2415,#2413,#325,.T.);
#3055=EDGE_CURVE('',#2412,#2414,#326,.T.);
#3056=EDGE_CURVE('',#2416,#2417,#1501,.T.);
#3057=EDGE_CURVE('',#2417,#2415,#327,.T.);
#3058=EDGE_CURVE('',#2414,#2416,#328,.T.);
#3059=EDGE_CURVE('',#2418,#2419,#1502,.T.);
#3060=EDGE_CURVE('',#2418,#2420,#329,.T.);
#3061=EDGE_CURVE('',#2421,#2420,#2007,.T.);
#3062=EDGE_CURVE('',#2421,#2419,#330,.T.);
#3063=EDGE_CURVE('',#2422,#2423,#1503,.T.);
#3064=EDGE_CURVE('',#2423,#2424,#331,.T.);
#3065=EDGE_CURVE('',#2425,#2424,#2008,.T.);
#3066=EDGE_CURVE('',#2422,#2425,#332,.T.);
#3067=EDGE_CURVE('',#2426,#2427,#1504,.T.);
#3068=EDGE_CURVE('',#2427,#2423,#333,.T.);
#3069=EDGE_CURVE('',#2426,#2422,#334,.T.);
#3070=EDGE_CURVE('',#2428,#2429,#1505,.T.);
#3071=EDGE_CURVE('',#2429,#2427,#335,.T.);
#3072=EDGE_CURVE('',#2428,#2426,#336,.T.);
#3073=EDGE_CURVE('',#2430,#2431,#1506,.T.);
#3074=EDGE_CURVE('',#2431,#2429,#337,.T.);
#3075=EDGE_CURVE('',#2430,#2428,#338,.T.);
#3076=EDGE_CURVE('',#2432,#2433,#1507,.T.);
#3077=EDGE_CURVE('',#2433,#2431,#339,.T.);
#3078=EDGE_CURVE('',#2432,#2430,#340,.T.);
#3079=EDGE_CURVE('',#2434,#2435,#1508,.T.);
#3080=EDGE_CURVE('',#2436,#2434,#341,.T.);
#3081=EDGE_CURVE('',#2437,#2436,#2009,.T.);
#3082=EDGE_CURVE('',#2437,#2435,#342,.T.);
#3083=EDGE_CURVE('',#2435,#2433,#343,.T.);
#3084=EDGE_CURVE('',#2434,#2432,#344,.T.);
#3085=EDGE_CURVE('',#2424,#2408,#345,.T.);
#3086=EDGE_CURVE('',#2420,#2437,#346,.T.);
#3087=EDGE_CURVE('',#2416,#2418,#347,.T.);
#3088=EDGE_CURVE('',#2411,#2425,#348,.T.);
#3089=EDGE_CURVE('',#2419,#2417,#349,.T.);
#3090=EDGE_CURVE('',#2436,#2421,#350,.T.);
#3091=EDGE_CURVE('',#2438,#2439,#1509,.T.);
#3092=EDGE_CURVE('',#2439,#2440,#1510,.T.);
#3093=EDGE_CURVE('',#2440,#2441,#1511,.T.);
#3094=EDGE_CURVE('',#2441,#2442,#1512,.T.);
#3095=EDGE_CURVE('',#2442,#2443,#1513,.T.);
#3096=EDGE_CURVE('',#2443,#2438,#1514,.T.);
#3097=EDGE_CURVE('',#2444,#2445,#1515,.T.);
#3098=EDGE_CURVE('',#2445,#2438,#1516,.T.);
#3099=EDGE_CURVE('',#2444,#2443,#1517,.T.);
#3100=EDGE_CURVE('',#2446,#2444,#1518,.T.);
#3101=EDGE_CURVE('',#2446,#2442,#1519,.T.);
#3102=EDGE_CURVE('',#2447,#2446,#1520,.T.);
#3103=EDGE_CURVE('',#2447,#2441,#1521,.T.);
#3104=EDGE_CURVE('',#2448,#2447,#1522,.T.);
#3105=EDGE_CURVE('',#2448,#2440,#1523,.T.);
#3106=EDGE_CURVE('',#2449,#2448,#1524,.T.);
#3107=EDGE_CURVE('',#2449,#2439,#1525,.T.);
#3108=EDGE_CURVE('',#2445,#2449,#1526,.T.);
#3109=EDGE_CURVE('',#2450,#2450,#2010,.T.);
#3110=EDGE_CURVE('',#2450,#2451,#1527,.T.);
#3111=EDGE_CURVE('',#2451,#2451,#2011,.T.);
#3112=ORIENTED_EDGE('',*,*,#2452,.F.);
#3113=ORIENTED_EDGE('',*,*,#2453,.T.);
#3114=ORIENTED_EDGE('',*,*,#2454,.T.);
#3115=ORIENTED_EDGE('',*,*,#2453,.F.);
#3116=ORIENTED_EDGE('',*,*,#2454,.F.);
#3117=ORIENTED_EDGE('',*,*,#2455,.F.);
#3118=ORIENTED_EDGE('',*,*,#2456,.F.);
#3119=ORIENTED_EDGE('',*,*,#2457,.T.);
#3120=ORIENTED_EDGE('',*,*,#2458,.T.);
#3121=ORIENTED_EDGE('',*,*,#2457,.F.);
#3122=ORIENTED_EDGE('',*,*,#2458,.F.);
#3123=ORIENTED_EDGE('',*,*,#2459,.F.);
#3124=ORIENTED_EDGE('',*,*,#2460,.F.);
#3125=ORIENTED_EDGE('',*,*,#2461,.T.);
#3126=ORIENTED_EDGE('',*,*,#2462,.T.);
#3127=ORIENTED_EDGE('',*,*,#2461,.F.);
#3128=ORIENTED_EDGE('',*,*,#2462,.F.);
#3129=ORIENTED_EDGE('',*,*,#2463,.F.);
#3130=ORIENTED_EDGE('',*,*,#2464,.T.);
#3131=ORIENTED_EDGE('',*,*,#2465,.T.);
#3132=ORIENTED_EDGE('',*,*,#2464,.F.);
#3133=ORIENTED_EDGE('',*,*,#2465,.F.);
#3134=ORIENTED_EDGE('',*,*,#2466,.F.);
#3135=ORIENTED_EDGE('',*,*,#2467,.T.);
#3136=ORIENTED_EDGE('',*,*,#2468,.T.);
#3137=ORIENTED_EDGE('',*,*,#2467,.F.);
#3138=ORIENTED_EDGE('',*,*,#2468,.F.);
#3139=ORIENTED_EDGE('',*,*,#2469,.F.);
#3140=ORIENTED_EDGE('',*,*,#2470,.T.);
#3141=ORIENTED_EDGE('',*,*,#2471,.T.);
#3142=ORIENTED_EDGE('',*,*,#2470,.F.);
#3143=ORIENTED_EDGE('',*,*,#2471,.F.);
#3144=ORIENTED_EDGE('',*,*,#2472,.F.);
#3145=ORIENTED_EDGE('',*,*,#2473,.T.);
#3146=ORIENTED_EDGE('',*,*,#2455,.T.);
#3147=ORIENTED_EDGE('',*,*,#2473,.F.);
#3148=ORIENTED_EDGE('',*,*,#2474,.F.);
#3149=ORIENTED_EDGE('',*,*,#2475,.T.);
#3150=ORIENTED_EDGE('',*,*,#2459,.T.);
#3151=ORIENTED_EDGE('',*,*,#2475,.F.);
#3152=ORIENTED_EDGE('',*,*,#2476,.F.);
#3153=ORIENTED_EDGE('',*,*,#2477,.F.);
#3154=ORIENTED_EDGE('',*,*,#2478,.F.);
#3155=ORIENTED_EDGE('',*,*,#2479,.F.);
#3156=ORIENTED_EDGE('',*,*,#2480,.F.);
#3157=ORIENTED_EDGE('',*,*,#2481,.F.);
#3158=ORIENTED_EDGE('',*,*,#2482,.F.);
#3159=ORIENTED_EDGE('',*,*,#2483,.F.);
#3160=ORIENTED_EDGE('',*,*,#2484,.F.);
#3161=ORIENTED_EDGE('',*,*,#2485,.F.);
#3162=ORIENTED_EDGE('',*,*,#2486,.F.);
#3163=ORIENTED_EDGE('',*,*,#2487,.T.);
#3164=ORIENTED_EDGE('',*,*,#2488,.F.);
#3165=ORIENTED_EDGE('',*,*,#2489,.F.);
#3166=ORIENTED_EDGE('',*,*,#2490,.F.);
#3167=ORIENTED_EDGE('',*,*,#2491,.T.);
#3168=ORIENTED_EDGE('',*,*,#2492,.F.);
#3169=ORIENTED_EDGE('',*,*,#2493,.F.);
#3170=ORIENTED_EDGE('',*,*,#2494,.F.);
#3171=ORIENTED_EDGE('',*,*,#2495,.F.);
#3172=ORIENTED_EDGE('',*,*,#2496,.F.);
#3173=ORIENTED_EDGE('',*,*,#2491,.F.);
#3174=ORIENTED_EDGE('',*,*,#2497,.T.);
#3175=ORIENTED_EDGE('',*,*,#2498,.F.);
#3176=ORIENTED_EDGE('',*,*,#2499,.F.);
#3177=ORIENTED_EDGE('',*,*,#2487,.F.);
#3178=ORIENTED_EDGE('',*,*,#2500,.T.);
#3179=ORIENTED_EDGE('',*,*,#2501,.F.);
#3180=ORIENTED_EDGE('',*,*,#2502,.F.);
#3181=ORIENTED_EDGE('',*,*,#2503,.F.);
#3182=ORIENTED_EDGE('',*,*,#2504,.T.);
#3183=ORIENTED_EDGE('',*,*,#2477,.T.);
#3184=ORIENTED_EDGE('',*,*,#2505,.F.);
#3185=ORIENTED_EDGE('',*,*,#2506,.F.);
#3186=ORIENTED_EDGE('',*,*,#2507,.T.);
#3187=ORIENTED_EDGE('',*,*,#2481,.T.);
#3188=ORIENTED_EDGE('',*,*,#2488,.T.);
#3189=ORIENTED_EDGE('',*,*,#2496,.T.);
#3190=ORIENTED_EDGE('',*,*,#2508,.F.);
#3191=ORIENTED_EDGE('',*,*,#2509,.F.);
#3192=ORIENTED_EDGE('',*,*,#2480,.T.);
#3193=ORIENTED_EDGE('',*,*,#2510,.F.);
#3194=ORIENTED_EDGE('',*,*,#2511,.F.);
#3195=ORIENTED_EDGE('',*,*,#2492,.T.);
#3196=ORIENTED_EDGE('',*,*,#2489,.T.);
#3197=ORIENTED_EDGE('',*,*,#2509,.T.);
#3198=ORIENTED_EDGE('',*,*,#2512,.F.);
#3199=ORIENTED_EDGE('',*,*,#2513,.T.);
#3200=ORIENTED_EDGE('',*,*,#2474,.T.);
#3201=ORIENTED_EDGE('',*,*,#2483,.T.);
#3202=ORIENTED_EDGE('',*,*,#2514,.T.);
#3203=ORIENTED_EDGE('',*,*,#2515,.T.);
#3204=ORIENTED_EDGE('',*,*,#2510,.T.);
#3205=ORIENTED_EDGE('',*,*,#2490,.T.);
#3206=ORIENTED_EDGE('',*,*,#2513,.F.);
#3207=ORIENTED_EDGE('',*,*,#2516,.F.);
#3208=ORIENTED_EDGE('',*,*,#2497,.F.);
#3209=ORIENTED_EDGE('',*,*,#2482,.T.);
#3210=ORIENTED_EDGE('',*,*,#2507,.F.);
#3211=ORIENTED_EDGE('',*,*,#2517,.F.);
#3212=ORIENTED_EDGE('',*,*,#2514,.F.);
#3213=ORIENTED_EDGE('',*,*,#2484,.T.);
#3214=ORIENTED_EDGE('',*,*,#2499,.T.);
#3215=ORIENTED_EDGE('',*,*,#2518,.F.);
#3216=ORIENTED_EDGE('',*,*,#2519,.F.);
#3217=ORIENTED_EDGE('',*,*,#2476,.T.);
#3218=ORIENTED_EDGE('',*,*,#2520,.F.);
#3219=ORIENTED_EDGE('',*,*,#2521,.F.);
#3220=ORIENTED_EDGE('',*,*,#2505,.T.);
#3221=ORIENTED_EDGE('',*,*,#2485,.T.);
#3222=ORIENTED_EDGE('',*,*,#2519,.T.);
#3223=ORIENTED_EDGE('',*,*,#2522,.F.);
#3224=ORIENTED_EDGE('',*,*,#2523,.T.);
#3225=ORIENTED_EDGE('',*,*,#2472,.T.);
#3226=ORIENTED_EDGE('',*,*,#2479,.T.);
#3227=ORIENTED_EDGE('',*,*,#2524,.T.);
#3228=ORIENTED_EDGE('',*,*,#2525,.T.);
#3229=ORIENTED_EDGE('',*,*,#2520,.T.);
#3230=ORIENTED_EDGE('',*,*,#2486,.T.);
#3231=ORIENTED_EDGE('',*,*,#2523,.F.);
#3232=ORIENTED_EDGE('',*,*,#2526,.F.);
#3233=ORIENTED_EDGE('',*,*,#2500,.F.);
#3234=ORIENTED_EDGE('',*,*,#2478,.T.);
#3235=ORIENTED_EDGE('',*,*,#2504,.F.);
#3236=ORIENTED_EDGE('',*,*,#2527,.F.);
#3237=ORIENTED_EDGE('',*,*,#2524,.F.);
#3238=ORIENTED_EDGE('',*,*,#2517,.T.);
#3239=ORIENTED_EDGE('',*,*,#2506,.T.);
#3240=ORIENTED_EDGE('',*,*,#2521,.T.);
#3241=ORIENTED_EDGE('',*,*,#2525,.F.);
#3242=ORIENTED_EDGE('',*,*,#2527,.T.);
#3243=ORIENTED_EDGE('',*,*,#2503,.T.);
#3244=ORIENTED_EDGE('',*,*,#2528,.T.);
#3245=ORIENTED_EDGE('',*,*,#2529,.T.);
#3246=ORIENTED_EDGE('',*,*,#2530,.F.);
#3247=ORIENTED_EDGE('',*,*,#2493,.T.);
#3248=ORIENTED_EDGE('',*,*,#2511,.T.);
#3249=ORIENTED_EDGE('',*,*,#2515,.F.);
#3250=ORIENTED_EDGE('',*,*,#2502,.T.);
#3251=ORIENTED_EDGE('',*,*,#2531,.F.);
#3252=ORIENTED_EDGE('',*,*,#2532,.F.);
#3253=ORIENTED_EDGE('',*,*,#2528,.F.);
#3254=ORIENTED_EDGE('',*,*,#2516,.T.);
#3255=ORIENTED_EDGE('',*,*,#2512,.T.);
#3256=ORIENTED_EDGE('',*,*,#2508,.T.);
#3257=ORIENTED_EDGE('',*,*,#2495,.T.);
#3258=ORIENTED_EDGE('',*,*,#2533,.F.);
#3259=ORIENTED_EDGE('',*,*,#2534,.F.);
#3260=ORIENTED_EDGE('',*,*,#2531,.T.);
#3261=ORIENTED_EDGE('',*,*,#2501,.T.);
#3262=ORIENTED_EDGE('',*,*,#2526,.T.);
#3263=ORIENTED_EDGE('',*,*,#2522,.T.);
#3264=ORIENTED_EDGE('',*,*,#2518,.T.);
#3265=ORIENTED_EDGE('',*,*,#2498,.T.);
#3266=ORIENTED_EDGE('',*,*,#2532,.T.);
#3267=ORIENTED_EDGE('',*,*,#2534,.T.);
#3268=ORIENTED_EDGE('',*,*,#2535,.F.);
#3269=ORIENTED_EDGE('',*,*,#2529,.F.);
#3270=ORIENTED_EDGE('',*,*,#2460,.T.);
#3271=ORIENTED_EDGE('',*,*,#2463,.T.);
#3272=ORIENTED_EDGE('',*,*,#2466,.T.);
#3273=ORIENTED_EDGE('',*,*,#2469,.T.);
#3274=ORIENTED_EDGE('',*,*,#2456,.T.);
#3275=ORIENTED_EDGE('',*,*,#2452,.T.);
#3276=ORIENTED_EDGE('',*,*,#2494,.T.);
#3277=ORIENTED_EDGE('',*,*,#2530,.T.);
#3278=ORIENTED_EDGE('',*,*,#2535,.T.);
#3279=ORIENTED_EDGE('',*,*,#2533,.T.);
#3280=ORIENTED_EDGE('',*,*,#2536,.F.);
#3281=ORIENTED_EDGE('',*,*,#2537,.T.);
#3282=ORIENTED_EDGE('',*,*,#2538,.T.);
#3283=ORIENTED_EDGE('',*,*,#2537,.F.);
#3284=ORIENTED_EDGE('',*,*,#2538,.F.);
#3285=ORIENTED_EDGE('',*,*,#2539,.F.);
#3286=ORIENTED_EDGE('',*,*,#2540,.T.);
#3287=ORIENTED_EDGE('',*,*,#2541,.T.);
#3288=ORIENTED_EDGE('',*,*,#2540,.F.);
#3289=ORIENTED_EDGE('',*,*,#2541,.F.);
#3290=ORIENTED_EDGE('',*,*,#2542,.F.);
#3291=ORIENTED_EDGE('',*,*,#2543,.T.);
#3292=ORIENTED_EDGE('',*,*,#2544,.T.);
#3293=ORIENTED_EDGE('',*,*,#2543,.F.);
#3294=ORIENTED_EDGE('',*,*,#2544,.F.);
#3295=ORIENTED_EDGE('',*,*,#2545,.F.);
#3296=ORIENTED_EDGE('',*,*,#2546,.T.);
#3297=ORIENTED_EDGE('',*,*,#2547,.T.);
#3298=ORIENTED_EDGE('',*,*,#2546,.F.);
#3299=ORIENTED_EDGE('',*,*,#2547,.F.);
#3300=ORIENTED_EDGE('',*,*,#2548,.F.);
#3301=ORIENTED_EDGE('',*,*,#2549,.T.);
#3302=ORIENTED_EDGE('',*,*,#2550,.F.);
#3303=ORIENTED_EDGE('',*,*,#2549,.F.);
#3304=ORIENTED_EDGE('',*,*,#2551,.F.);
#3305=ORIENTED_EDGE('',*,*,#2552,.T.);
#3306=ORIENTED_EDGE('',*,*,#2553,.F.);
#3307=ORIENTED_EDGE('',*,*,#2552,.F.);
#3308=ORIENTED_EDGE('',*,*,#2554,.F.);
#3309=ORIENTED_EDGE('',*,*,#2555,.F.);
#3310=ORIENTED_EDGE('',*,*,#2556,.F.);
#3311=ORIENTED_EDGE('',*,*,#2557,.F.);
#3312=ORIENTED_EDGE('',*,*,#2558,.F.);
#3313=ORIENTED_EDGE('',*,*,#2559,.F.);
#3314=ORIENTED_EDGE('',*,*,#2560,.F.);
#3315=ORIENTED_EDGE('',*,*,#2561,.F.);
#3316=ORIENTED_EDGE('',*,*,#2562,.F.);
#3317=ORIENTED_EDGE('',*,*,#2563,.F.);
#3318=ORIENTED_EDGE('',*,*,#2564,.F.);
#3319=ORIENTED_EDGE('',*,*,#2565,.T.);
#3320=ORIENTED_EDGE('',*,*,#2566,.F.);
#3321=ORIENTED_EDGE('',*,*,#2567,.F.);
#3322=ORIENTED_EDGE('',*,*,#2568,.F.);
#3323=ORIENTED_EDGE('',*,*,#2569,.T.);
#3324=ORIENTED_EDGE('',*,*,#2570,.F.);
#3325=ORIENTED_EDGE('',*,*,#2571,.F.);
#3326=ORIENTED_EDGE('',*,*,#2572,.F.);
#3327=ORIENTED_EDGE('',*,*,#2573,.F.);
#3328=ORIENTED_EDGE('',*,*,#2574,.F.);
#3329=ORIENTED_EDGE('',*,*,#2569,.F.);
#3330=ORIENTED_EDGE('',*,*,#2575,.T.);
#3331=ORIENTED_EDGE('',*,*,#2576,.F.);
#3332=ORIENTED_EDGE('',*,*,#2577,.F.);
#3333=ORIENTED_EDGE('',*,*,#2565,.F.);
#3334=ORIENTED_EDGE('',*,*,#2578,.T.);
#3335=ORIENTED_EDGE('',*,*,#2579,.F.);
#3336=ORIENTED_EDGE('',*,*,#2580,.F.);
#3337=ORIENTED_EDGE('',*,*,#2581,.F.);
#3338=ORIENTED_EDGE('',*,*,#2582,.T.);
#3339=ORIENTED_EDGE('',*,*,#2555,.T.);
#3340=ORIENTED_EDGE('',*,*,#2583,.F.);
#3341=ORIENTED_EDGE('',*,*,#2584,.F.);
#3342=ORIENTED_EDGE('',*,*,#2585,.T.);
#3343=ORIENTED_EDGE('',*,*,#2559,.T.);
#3344=ORIENTED_EDGE('',*,*,#2566,.T.);
#3345=ORIENTED_EDGE('',*,*,#2574,.T.);
#3346=ORIENTED_EDGE('',*,*,#2586,.F.);
#3347=ORIENTED_EDGE('',*,*,#2587,.F.);
#3348=ORIENTED_EDGE('',*,*,#2558,.T.);
#3349=ORIENTED_EDGE('',*,*,#2588,.F.);
#3350=ORIENTED_EDGE('',*,*,#2589,.F.);
#3351=ORIENTED_EDGE('',*,*,#2570,.T.);
#3352=ORIENTED_EDGE('',*,*,#2567,.T.);
#3353=ORIENTED_EDGE('',*,*,#2587,.T.);
#3354=ORIENTED_EDGE('',*,*,#2590,.F.);
#3355=ORIENTED_EDGE('',*,*,#2591,.T.);
#3356=ORIENTED_EDGE('',*,*,#2551,.T.);
#3357=ORIENTED_EDGE('',*,*,#2561,.T.);
#3358=ORIENTED_EDGE('',*,*,#2592,.T.);
#3359=ORIENTED_EDGE('',*,*,#2593,.T.);
#3360=ORIENTED_EDGE('',*,*,#2588,.T.);
#3361=ORIENTED_EDGE('',*,*,#2568,.T.);
#3362=ORIENTED_EDGE('',*,*,#2591,.F.);
#3363=ORIENTED_EDGE('',*,*,#2594,.F.);
#3364=ORIENTED_EDGE('',*,*,#2575,.F.);
#3365=ORIENTED_EDGE('',*,*,#2560,.T.);
#3366=ORIENTED_EDGE('',*,*,#2585,.F.);
#3367=ORIENTED_EDGE('',*,*,#2595,.F.);
#3368=ORIENTED_EDGE('',*,*,#2592,.F.);
#3369=ORIENTED_EDGE('',*,*,#2562,.T.);
#3370=ORIENTED_EDGE('',*,*,#2577,.T.);
#3371=ORIENTED_EDGE('',*,*,#2596,.F.);
#3372=ORIENTED_EDGE('',*,*,#2597,.F.);
#3373=ORIENTED_EDGE('',*,*,#2554,.T.);
#3374=ORIENTED_EDGE('',*,*,#2598,.F.);
#3375=ORIENTED_EDGE('',*,*,#2599,.F.);
#3376=ORIENTED_EDGE('',*,*,#2583,.T.);
#3377=ORIENTED_EDGE('',*,*,#2563,.T.);
#3378=ORIENTED_EDGE('',*,*,#2597,.T.);
#3379=ORIENTED_EDGE('',*,*,#2600,.F.);
#3380=ORIENTED_EDGE('',*,*,#2601,.T.);
#3381=ORIENTED_EDGE('',*,*,#2548,.T.);
#3382=ORIENTED_EDGE('',*,*,#2557,.T.);
#3383=ORIENTED_EDGE('',*,*,#2602,.T.);
#3384=ORIENTED_EDGE('',*,*,#2603,.T.);
#3385=ORIENTED_EDGE('',*,*,#2598,.T.);
#3386=ORIENTED_EDGE('',*,*,#2564,.T.);
#3387=ORIENTED_EDGE('',*,*,#2601,.F.);
#3388=ORIENTED_EDGE('',*,*,#2604,.F.);
#3389=ORIENTED_EDGE('',*,*,#2578,.F.);
#3390=ORIENTED_EDGE('',*,*,#2556,.T.);
#3391=ORIENTED_EDGE('',*,*,#2582,.F.);
#3392=ORIENTED_EDGE('',*,*,#2605,.F.);
#3393=ORIENTED_EDGE('',*,*,#2602,.F.);
#3394=ORIENTED_EDGE('',*,*,#2595,.T.);
#3395=ORIENTED_EDGE('',*,*,#2584,.T.);
#3396=ORIENTED_EDGE('',*,*,#2599,.T.);
#3397=ORIENTED_EDGE('',*,*,#2603,.F.);
#3398=ORIENTED_EDGE('',*,*,#2605,.T.);
#3399=ORIENTED_EDGE('',*,*,#2581,.T.);
#3400=ORIENTED_EDGE('',*,*,#2606,.T.);
#3401=ORIENTED_EDGE('',*,*,#2607,.T.);
#3402=ORIENTED_EDGE('',*,*,#2608,.F.);
#3403=ORIENTED_EDGE('',*,*,#2571,.T.);
#3404=ORIENTED_EDGE('',*,*,#2589,.T.);
#3405=ORIENTED_EDGE('',*,*,#2593,.F.);
#3406=ORIENTED_EDGE('',*,*,#2580,.T.);
#3407=ORIENTED_EDGE('',*,*,#2609,.F.);
#3408=ORIENTED_EDGE('',*,*,#2610,.F.);
#3409=ORIENTED_EDGE('',*,*,#2606,.F.);
#3410=ORIENTED_EDGE('',*,*,#2594,.T.);
#3411=ORIENTED_EDGE('',*,*,#2590,.T.);
#3412=ORIENTED_EDGE('',*,*,#2586,.T.);
#3413=ORIENTED_EDGE('',*,*,#2573,.T.);
#3414=ORIENTED_EDGE('',*,*,#2611,.F.);
#3415=ORIENTED_EDGE('',*,*,#2612,.F.);
#3416=ORIENTED_EDGE('',*,*,#2609,.T.);
#3417=ORIENTED_EDGE('',*,*,#2579,.T.);
#3418=ORIENTED_EDGE('',*,*,#2604,.T.);
#3419=ORIENTED_EDGE('',*,*,#2600,.T.);
#3420=ORIENTED_EDGE('',*,*,#2596,.T.);
#3421=ORIENTED_EDGE('',*,*,#2576,.T.);
#3422=ORIENTED_EDGE('',*,*,#2610,.T.);
#3423=ORIENTED_EDGE('',*,*,#2612,.T.);
#3424=ORIENTED_EDGE('',*,*,#2613,.F.);
#3425=ORIENTED_EDGE('',*,*,#2607,.F.);
#3426=ORIENTED_EDGE('',*,*,#2553,.T.);
#3427=ORIENTED_EDGE('',*,*,#2550,.T.);
#3428=ORIENTED_EDGE('',*,*,#2545,.T.);
#3429=ORIENTED_EDGE('',*,*,#2542,.T.);
#3430=ORIENTED_EDGE('',*,*,#2539,.T.);
#3431=ORIENTED_EDGE('',*,*,#2536,.T.);
#3432=ORIENTED_EDGE('',*,*,#2572,.T.);
#3433=ORIENTED_EDGE('',*,*,#2608,.T.);
#3434=ORIENTED_EDGE('',*,*,#2613,.T.);
#3435=ORIENTED_EDGE('',*,*,#2611,.T.);
#3436=ORIENTED_EDGE('',*,*,#2614,.F.);
#3437=ORIENTED_EDGE('',*,*,#2615,.F.);
#3438=ORIENTED_EDGE('',*,*,#2616,.F.);
#3439=ORIENTED_EDGE('',*,*,#2617,.F.);
#3440=ORIENTED_EDGE('',*,*,#2618,.F.);
#3441=ORIENTED_EDGE('',*,*,#2619,.F.);
#3442=ORIENTED_EDGE('',*,*,#2620,.F.);
#3443=ORIENTED_EDGE('',*,*,#2621,.F.);
#3444=ORIENTED_EDGE('',*,*,#2622,.F.);
#3445=ORIENTED_EDGE('',*,*,#2616,.T.);
#3446=ORIENTED_EDGE('',*,*,#2623,.F.);
#3447=ORIENTED_EDGE('',*,*,#2620,.T.);
#3448=ORIENTED_EDGE('',*,*,#2621,.T.);
#3449=ORIENTED_EDGE('',*,*,#2623,.T.);
#3450=ORIENTED_EDGE('',*,*,#2615,.T.);
#3451=ORIENTED_EDGE('',*,*,#2624,.F.);
#3452=ORIENTED_EDGE('',*,*,#2625,.F.);
#3453=ORIENTED_EDGE('',*,*,#2626,.T.);
#3454=ORIENTED_EDGE('',*,*,#2627,.T.);
#3455=ORIENTED_EDGE('',*,*,#2628,.F.);
#3456=ORIENTED_EDGE('',*,*,#2614,.T.);
#3457=ORIENTED_EDGE('',*,*,#2629,.T.);
#3458=ORIENTED_EDGE('',*,*,#2630,.T.);
#3459=ORIENTED_EDGE('',*,*,#2624,.T.);
#3460=ORIENTED_EDGE('',*,*,#2631,.T.);
#3461=ORIENTED_EDGE('',*,*,#2632,.T.);
#3462=ORIENTED_EDGE('',*,*,#2633,.F.);
#3463=ORIENTED_EDGE('',*,*,#2627,.F.);
#3464=ORIENTED_EDGE('',*,*,#2634,.T.);
#3465=ORIENTED_EDGE('',*,*,#2625,.T.);
#3466=ORIENTED_EDGE('',*,*,#2630,.F.);
#3467=ORIENTED_EDGE('',*,*,#2635,.F.);
#3468=ORIENTED_EDGE('',*,*,#2619,.T.);
#3469=ORIENTED_EDGE('',*,*,#2636,.F.);
#3470=ORIENTED_EDGE('',*,*,#2632,.F.);
#3471=ORIENTED_EDGE('',*,*,#2637,.T.);
#3472=ORIENTED_EDGE('',*,*,#2635,.T.);
#3473=ORIENTED_EDGE('',*,*,#2629,.F.);
#3474=ORIENTED_EDGE('',*,*,#2617,.T.);
#3475=ORIENTED_EDGE('',*,*,#2622,.T.);
#3476=ORIENTED_EDGE('',*,*,#2618,.T.);
#3477=ORIENTED_EDGE('',*,*,#2628,.T.);
#3478=ORIENTED_EDGE('',*,*,#2633,.T.);
#3479=ORIENTED_EDGE('',*,*,#2636,.T.);
#3480=ORIENTED_EDGE('',*,*,#2637,.F.);
#3481=ORIENTED_EDGE('',*,*,#2631,.F.);
#3482=ORIENTED_EDGE('',*,*,#2626,.F.);
#3483=ORIENTED_EDGE('',*,*,#2634,.F.);
#3484=ORIENTED_EDGE('',*,*,#2638,.T.);
#3485=ORIENTED_EDGE('',*,*,#2639,.T.);
#3486=ORIENTED_EDGE('',*,*,#2640,.F.);
#3487=ORIENTED_EDGE('',*,*,#2641,.F.);
#3488=ORIENTED_EDGE('',*,*,#2642,.T.);
#3489=ORIENTED_EDGE('',*,*,#2641,.T.);
#3490=ORIENTED_EDGE('',*,*,#2643,.F.);
#3491=ORIENTED_EDGE('',*,*,#2644,.F.);
#3492=ORIENTED_EDGE('',*,*,#2645,.T.);
#3493=ORIENTED_EDGE('',*,*,#2644,.T.);
#3494=ORIENTED_EDGE('',*,*,#2646,.F.);
#3495=ORIENTED_EDGE('',*,*,#2647,.F.);
#3496=ORIENTED_EDGE('',*,*,#2648,.T.);
#3497=ORIENTED_EDGE('',*,*,#2647,.T.);
#3498=ORIENTED_EDGE('',*,*,#2649,.F.);
#3499=ORIENTED_EDGE('',*,*,#2639,.F.);
#3500=ORIENTED_EDGE('',*,*,#2649,.T.);
#3501=ORIENTED_EDGE('',*,*,#2646,.T.);
#3502=ORIENTED_EDGE('',*,*,#2643,.T.);
#3503=ORIENTED_EDGE('',*,*,#2640,.T.);
#3504=ORIENTED_EDGE('',*,*,#2648,.F.);
#3505=ORIENTED_EDGE('',*,*,#2638,.F.);
#3506=ORIENTED_EDGE('',*,*,#2642,.F.);
#3507=ORIENTED_EDGE('',*,*,#2645,.F.);
#3508=ORIENTED_EDGE('',*,*,#2650,.F.);
#3509=ORIENTED_EDGE('',*,*,#2651,.T.);
#3510=ORIENTED_EDGE('',*,*,#2652,.F.);
#3511=ORIENTED_EDGE('',*,*,#2653,.F.);
#3512=ORIENTED_EDGE('',*,*,#2654,.F.);
#3513=ORIENTED_EDGE('',*,*,#2655,.F.);
#3514=ORIENTED_EDGE('',*,*,#2656,.F.);
#3515=ORIENTED_EDGE('',*,*,#2651,.F.);
#3516=ORIENTED_EDGE('',*,*,#2653,.T.);
#3517=ORIENTED_EDGE('',*,*,#2657,.F.);
#3518=ORIENTED_EDGE('',*,*,#2658,.F.);
#3519=ORIENTED_EDGE('',*,*,#2659,.T.);
#3520=ORIENTED_EDGE('',*,*,#2655,.T.);
#3521=ORIENTED_EDGE('',*,*,#2660,.T.);
#3522=ORIENTED_EDGE('',*,*,#2661,.T.);
#3523=ORIENTED_EDGE('',*,*,#2662,.F.);
#3524=ORIENTED_EDGE('',*,*,#2663,.T.);
#3525=ORIENTED_EDGE('',*,*,#2658,.T.);
#3526=ORIENTED_EDGE('',*,*,#2664,.F.);
#3527=ORIENTED_EDGE('',*,*,#2665,.F.);
#3528=ORIENTED_EDGE('',*,*,#2666,.T.);
#3529=ORIENTED_EDGE('',*,*,#2665,.T.);
#3530=ORIENTED_EDGE('',*,*,#2667,.F.);
#3531=ORIENTED_EDGE('',*,*,#2661,.F.);
#3532=ORIENTED_EDGE('',*,*,#2656,.T.);
#3533=ORIENTED_EDGE('',*,*,#2662,.T.);
#3534=ORIENTED_EDGE('',*,*,#2667,.T.);
#3535=ORIENTED_EDGE('',*,*,#2664,.T.);
#3536=ORIENTED_EDGE('',*,*,#2657,.T.);
#3537=ORIENTED_EDGE('',*,*,#2652,.T.);
#3538=ORIENTED_EDGE('',*,*,#2650,.T.);
#3539=ORIENTED_EDGE('',*,*,#2659,.F.);
#3540=ORIENTED_EDGE('',*,*,#2663,.F.);
#3541=ORIENTED_EDGE('',*,*,#2666,.F.);
#3542=ORIENTED_EDGE('',*,*,#2660,.F.);
#3543=ORIENTED_EDGE('',*,*,#2654,.T.);
#3544=ORIENTED_EDGE('',*,*,#2668,.F.);
#3545=ORIENTED_EDGE('',*,*,#2669,.T.);
#3546=ORIENTED_EDGE('',*,*,#2670,.F.);
#3547=ORIENTED_EDGE('',*,*,#2671,.F.);
#3548=ORIENTED_EDGE('',*,*,#2672,.F.);
#3549=ORIENTED_EDGE('',*,*,#2673,.T.);
#3550=ORIENTED_EDGE('',*,*,#2674,.F.);
#3551=ORIENTED_EDGE('',*,*,#2669,.F.);
#3552=ORIENTED_EDGE('',*,*,#2675,.F.);
#3553=ORIENTED_EDGE('',*,*,#2676,.T.);
#3554=ORIENTED_EDGE('',*,*,#2677,.F.);
#3555=ORIENTED_EDGE('',*,*,#2673,.F.);
#3556=ORIENTED_EDGE('',*,*,#2678,.F.);
#3557=ORIENTED_EDGE('',*,*,#2671,.T.);
#3558=ORIENTED_EDGE('',*,*,#2679,.F.);
#3559=ORIENTED_EDGE('',*,*,#2676,.F.);
#3560=ORIENTED_EDGE('',*,*,#2680,.F.);
#3561=ORIENTED_EDGE('',*,*,#2681,.T.);
#3562=ORIENTED_EDGE('',*,*,#2682,.F.);
#3563=ORIENTED_EDGE('',*,*,#2681,.F.);
#3564=ORIENTED_EDGE('',*,*,#2683,.F.);
#3565=ORIENTED_EDGE('',*,*,#2684,.T.);
#3566=ORIENTED_EDGE('',*,*,#2685,.F.);
#3567=ORIENTED_EDGE('',*,*,#2684,.F.);
#3568=ORIENTED_EDGE('',*,*,#2686,.T.);
#3569=ORIENTED_EDGE('',*,*,#2687,.T.);
#3570=ORIENTED_EDGE('',*,*,#2688,.F.);
#3571=ORIENTED_EDGE('',*,*,#2689,.F.);
#3572=ORIENTED_EDGE('',*,*,#2668,.T.);
#3573=ORIENTED_EDGE('',*,*,#2678,.T.);
#3574=ORIENTED_EDGE('',*,*,#2675,.T.);
#3575=ORIENTED_EDGE('',*,*,#2672,.T.);
#3576=ORIENTED_EDGE('',*,*,#2680,.T.);
#3577=ORIENTED_EDGE('',*,*,#2683,.T.);
#3578=ORIENTED_EDGE('',*,*,#2690,.T.);
#3579=ORIENTED_EDGE('',*,*,#2689,.T.);
#3580=ORIENTED_EDGE('',*,*,#2691,.F.);
#3581=ORIENTED_EDGE('',*,*,#2692,.F.);
#3582=ORIENTED_EDGE('',*,*,#2693,.T.);
#3583=ORIENTED_EDGE('',*,*,#2692,.T.);
#3584=ORIENTED_EDGE('',*,*,#2694,.F.);
#3585=ORIENTED_EDGE('',*,*,#2695,.F.);
#3586=ORIENTED_EDGE('',*,*,#2670,.T.);
#3587=ORIENTED_EDGE('',*,*,#2674,.T.);
#3588=ORIENTED_EDGE('',*,*,#2677,.T.);
#3589=ORIENTED_EDGE('',*,*,#2679,.T.);
#3590=ORIENTED_EDGE('',*,*,#2682,.T.);
#3591=ORIENTED_EDGE('',*,*,#2685,.T.);
#3592=ORIENTED_EDGE('',*,*,#2696,.T.);
#3593=ORIENTED_EDGE('',*,*,#2695,.T.);
#3594=ORIENTED_EDGE('',*,*,#2697,.F.);
#3595=ORIENTED_EDGE('',*,*,#2687,.F.);
#3596=ORIENTED_EDGE('',*,*,#2697,.T.);
#3597=ORIENTED_EDGE('',*,*,#2694,.T.);
#3598=ORIENTED_EDGE('',*,*,#2691,.T.);
#3599=ORIENTED_EDGE('',*,*,#2688,.T.);
#3600=ORIENTED_EDGE('',*,*,#2696,.F.);
#3601=ORIENTED_EDGE('',*,*,#2686,.F.);
#3602=ORIENTED_EDGE('',*,*,#2690,.F.);
#3603=ORIENTED_EDGE('',*,*,#2693,.F.);
#3604=ORIENTED_EDGE('',*,*,#2698,.F.);
#3605=ORIENTED_EDGE('',*,*,#2699,.T.);
#3606=ORIENTED_EDGE('',*,*,#2700,.F.);
#3607=ORIENTED_EDGE('',*,*,#2699,.F.);
#3608=ORIENTED_EDGE('',*,*,#2701,.F.);
#3609=ORIENTED_EDGE('',*,*,#2702,.T.);
#3610=ORIENTED_EDGE('',*,*,#2703,.F.);
#3611=ORIENTED_EDGE('',*,*,#2702,.F.);
#3612=ORIENTED_EDGE('',*,*,#2704,.F.);
#3613=ORIENTED_EDGE('',*,*,#2705,.F.);
#3614=ORIENTED_EDGE('',*,*,#2706,.F.);
#3615=ORIENTED_EDGE('',*,*,#2707,.F.);
#3616=ORIENTED_EDGE('',*,*,#2708,.F.);
#3617=ORIENTED_EDGE('',*,*,#2709,.F.);
#3618=ORIENTED_EDGE('',*,*,#2710,.F.);
#3619=ORIENTED_EDGE('',*,*,#2705,.T.);
#3620=ORIENTED_EDGE('',*,*,#2711,.F.);
#3621=ORIENTED_EDGE('',*,*,#2712,.F.);
#3622=ORIENTED_EDGE('',*,*,#2713,.F.);
#3623=ORIENTED_EDGE('',*,*,#2709,.T.);
#3624=ORIENTED_EDGE('',*,*,#2706,.T.);
#3625=ORIENTED_EDGE('',*,*,#2710,.T.);
#3626=ORIENTED_EDGE('',*,*,#2713,.T.);
#3627=ORIENTED_EDGE('',*,*,#2714,.F.);
#3628=ORIENTED_EDGE('',*,*,#2715,.T.);
#3629=ORIENTED_EDGE('',*,*,#2716,.T.);
#3630=ORIENTED_EDGE('',*,*,#2717,.T.);
#3631=ORIENTED_EDGE('',*,*,#2718,.T.);
#3632=ORIENTED_EDGE('',*,*,#2719,.F.);
#3633=ORIENTED_EDGE('',*,*,#2720,.T.);
#3634=ORIENTED_EDGE('',*,*,#2721,.T.);
#3635=ORIENTED_EDGE('',*,*,#2722,.F.);
#3636=ORIENTED_EDGE('',*,*,#2700,.T.);
#3637=ORIENTED_EDGE('',*,*,#2703,.T.);
#3638=ORIENTED_EDGE('',*,*,#2712,.T.);
#3639=ORIENTED_EDGE('',*,*,#2723,.F.);
#3640=ORIENTED_EDGE('',*,*,#2724,.T.);
#3641=ORIENTED_EDGE('',*,*,#2725,.T.);
#3642=ORIENTED_EDGE('',*,*,#2726,.T.);
#3643=ORIENTED_EDGE('',*,*,#2714,.T.);
#3644=ORIENTED_EDGE('',*,*,#2707,.T.);
#3645=ORIENTED_EDGE('',*,*,#2722,.T.);
#3646=ORIENTED_EDGE('',*,*,#2727,.T.);
#3647=ORIENTED_EDGE('',*,*,#2728,.T.);
#3648=ORIENTED_EDGE('',*,*,#2729,.F.);
#3649=ORIENTED_EDGE('',*,*,#2730,.F.);
#3650=ORIENTED_EDGE('',*,*,#2727,.F.);
#3651=ORIENTED_EDGE('',*,*,#2721,.F.);
#3652=ORIENTED_EDGE('',*,*,#2731,.F.);
#3653=ORIENTED_EDGE('',*,*,#2732,.F.);
#3654=ORIENTED_EDGE('',*,*,#2733,.F.);
#3655=ORIENTED_EDGE('',*,*,#2720,.F.);
#3656=ORIENTED_EDGE('',*,*,#2734,.F.);
#3657=ORIENTED_EDGE('',*,*,#2735,.F.);
#3658=ORIENTED_EDGE('',*,*,#2731,.T.);
#3659=ORIENTED_EDGE('',*,*,#2728,.F.);
#3660=ORIENTED_EDGE('',*,*,#2733,.T.);
#3661=ORIENTED_EDGE('',*,*,#2736,.F.);
#3662=ORIENTED_EDGE('',*,*,#2737,.F.);
#3663=ORIENTED_EDGE('',*,*,#2719,.T.);
#3664=ORIENTED_EDGE('',*,*,#2738,.T.);
#3665=ORIENTED_EDGE('',*,*,#2739,.T.);
#3666=ORIENTED_EDGE('',*,*,#2734,.T.);
#3667=ORIENTED_EDGE('',*,*,#2737,.T.);
#3668=ORIENTED_EDGE('',*,*,#2740,.T.);
#3669=ORIENTED_EDGE('',*,*,#2729,.T.);
#3670=ORIENTED_EDGE('',*,*,#2704,.T.);
#3671=ORIENTED_EDGE('',*,*,#2730,.T.);
#3672=ORIENTED_EDGE('',*,*,#2740,.F.);
#3673=ORIENTED_EDGE('',*,*,#2736,.T.);
#3674=ORIENTED_EDGE('',*,*,#2732,.T.);
#3675=ORIENTED_EDGE('',*,*,#2735,.T.);
#3676=ORIENTED_EDGE('',*,*,#2739,.F.);
#3677=ORIENTED_EDGE('',*,*,#2741,.F.);
#3678=ORIENTED_EDGE('',*,*,#2742,.T.);
#3679=ORIENTED_EDGE('',*,*,#2743,.T.);
#3680=ORIENTED_EDGE('',*,*,#2744,.T.);
#3681=ORIENTED_EDGE('',*,*,#2745,.T.);
#3682=ORIENTED_EDGE('',*,*,#2746,.T.);
#3683=ORIENTED_EDGE('',*,*,#2723,.T.);
#3684=ORIENTED_EDGE('',*,*,#2711,.T.);
#3685=ORIENTED_EDGE('',*,*,#2708,.T.);
#3686=ORIENTED_EDGE('',*,*,#2698,.T.);
#3687=ORIENTED_EDGE('',*,*,#2701,.T.);
#3688=ORIENTED_EDGE('',*,*,#2725,.F.);
#3689=ORIENTED_EDGE('',*,*,#2747,.T.);
#3690=ORIENTED_EDGE('',*,*,#2745,.F.);
#3691=ORIENTED_EDGE('',*,*,#2748,.F.);
#3692=ORIENTED_EDGE('',*,*,#2716,.F.);
#3693=ORIENTED_EDGE('',*,*,#2749,.F.);
#3694=ORIENTED_EDGE('',*,*,#2743,.F.);
#3695=ORIENTED_EDGE('',*,*,#2750,.T.);
#3696=ORIENTED_EDGE('',*,*,#2726,.F.);
#3697=ORIENTED_EDGE('',*,*,#2748,.T.);
#3698=ORIENTED_EDGE('',*,*,#2744,.F.);
#3699=ORIENTED_EDGE('',*,*,#2749,.T.);
#3700=ORIENTED_EDGE('',*,*,#2715,.F.);
#3701=ORIENTED_EDGE('',*,*,#2751,.T.);
#3702=ORIENTED_EDGE('',*,*,#2741,.T.);
#3703=ORIENTED_EDGE('',*,*,#2738,.F.);
#3704=ORIENTED_EDGE('',*,*,#2718,.F.);
#3705=ORIENTED_EDGE('',*,*,#2750,.F.);
#3706=ORIENTED_EDGE('',*,*,#2742,.F.);
#3707=ORIENTED_EDGE('',*,*,#2751,.F.);
#3708=ORIENTED_EDGE('',*,*,#2717,.F.);
#3709=ORIENTED_EDGE('',*,*,#2724,.F.);
#3710=ORIENTED_EDGE('',*,*,#2746,.F.);
#3711=ORIENTED_EDGE('',*,*,#2747,.F.);
#3712=ORIENTED_EDGE('',*,*,#2752,.F.);
#3713=ORIENTED_EDGE('',*,*,#2753,.T.);
#3714=ORIENTED_EDGE('',*,*,#2754,.F.);
#3715=ORIENTED_EDGE('',*,*,#2753,.F.);
#3716=ORIENTED_EDGE('',*,*,#2755,.F.);
#3717=ORIENTED_EDGE('',*,*,#2756,.T.);
#3718=ORIENTED_EDGE('',*,*,#2757,.F.);
#3719=ORIENTED_EDGE('',*,*,#2756,.F.);
#3720=ORIENTED_EDGE('',*,*,#2758,.F.);
#3721=ORIENTED_EDGE('',*,*,#2759,.T.);
#3722=ORIENTED_EDGE('',*,*,#2760,.F.);
#3723=ORIENTED_EDGE('',*,*,#2761,.F.);
#3724=ORIENTED_EDGE('',*,*,#2762,.F.);
#3725=ORIENTED_EDGE('',*,*,#2763,.F.);
#3726=ORIENTED_EDGE('',*,*,#2759,.F.);
#3727=ORIENTED_EDGE('',*,*,#2761,.T.);
#3728=ORIENTED_EDGE('',*,*,#2758,.T.);
#3729=ORIENTED_EDGE('',*,*,#2764,.F.);
#3730=ORIENTED_EDGE('',*,*,#2765,.T.);
#3731=ORIENTED_EDGE('',*,*,#2766,.T.);
#3732=ORIENTED_EDGE('',*,*,#2767,.T.);
#3733=ORIENTED_EDGE('',*,*,#2768,.F.);
#3734=ORIENTED_EDGE('',*,*,#2769,.T.);
#3735=ORIENTED_EDGE('',*,*,#2770,.T.);
#3736=ORIENTED_EDGE('',*,*,#2771,.T.);
#3737=ORIENTED_EDGE('',*,*,#2772,.T.);
#3738=ORIENTED_EDGE('',*,*,#2773,.F.);
#3739=ORIENTED_EDGE('',*,*,#2754,.T.);
#3740=ORIENTED_EDGE('',*,*,#2757,.T.);
#3741=ORIENTED_EDGE('',*,*,#2760,.T.);
#3742=ORIENTED_EDGE('',*,*,#2763,.T.);
#3743=ORIENTED_EDGE('',*,*,#2774,.F.);
#3744=ORIENTED_EDGE('',*,*,#2775,.F.);
#3745=ORIENTED_EDGE('',*,*,#2776,.T.);
#3746=ORIENTED_EDGE('',*,*,#2777,.T.);
#3747=ORIENTED_EDGE('',*,*,#2778,.T.);
#3748=ORIENTED_EDGE('',*,*,#2768,.T.);
#3749=ORIENTED_EDGE('',*,*,#2779,.T.);
#3750=ORIENTED_EDGE('',*,*,#2780,.T.);
#3751=ORIENTED_EDGE('',*,*,#2781,.T.);
#3752=ORIENTED_EDGE('',*,*,#2764,.T.);
#3753=ORIENTED_EDGE('',*,*,#2770,.F.);
#3754=ORIENTED_EDGE('',*,*,#2782,.T.);
#3755=ORIENTED_EDGE('',*,*,#2777,.F.);
#3756=ORIENTED_EDGE('',*,*,#2783,.F.);
#3757=ORIENTED_EDGE('',*,*,#2769,.F.);
#3758=ORIENTED_EDGE('',*,*,#2778,.F.);
#3759=ORIENTED_EDGE('',*,*,#2782,.F.);
#3760=ORIENTED_EDGE('',*,*,#2783,.T.);
#3761=ORIENTED_EDGE('',*,*,#2776,.F.);
#3762=ORIENTED_EDGE('',*,*,#2784,.F.);
#3763=ORIENTED_EDGE('',*,*,#2785,.F.);
#3764=ORIENTED_EDGE('',*,*,#2771,.F.);
#3765=ORIENTED_EDGE('',*,*,#2765,.F.);
#3766=ORIENTED_EDGE('',*,*,#2781,.F.);
#3767=ORIENTED_EDGE('',*,*,#2786,.T.);
#3768=ORIENTED_EDGE('',*,*,#2787,.T.);
#3769=ORIENTED_EDGE('',*,*,#2787,.F.);
#3770=ORIENTED_EDGE('',*,*,#2788,.T.);
#3771=ORIENTED_EDGE('',*,*,#2789,.T.);
#3772=ORIENTED_EDGE('',*,*,#2788,.F.);
#3773=ORIENTED_EDGE('',*,*,#2766,.F.);
#3774=ORIENTED_EDGE('',*,*,#2786,.F.);
#3775=ORIENTED_EDGE('',*,*,#2780,.F.);
#3776=ORIENTED_EDGE('',*,*,#2790,.T.);
#3777=ORIENTED_EDGE('',*,*,#2767,.F.);
#3778=ORIENTED_EDGE('',*,*,#2790,.F.);
#3779=ORIENTED_EDGE('',*,*,#2779,.F.);
#3780=ORIENTED_EDGE('',*,*,#2789,.F.);
#3781=ORIENTED_EDGE('',*,*,#2784,.T.);
#3782=ORIENTED_EDGE('',*,*,#2775,.T.);
#3783=ORIENTED_EDGE('',*,*,#2791,.F.);
#3784=ORIENTED_EDGE('',*,*,#2792,.F.);
#3785=ORIENTED_EDGE('',*,*,#2752,.T.);
#3786=ORIENTED_EDGE('',*,*,#2755,.T.);
#3787=ORIENTED_EDGE('',*,*,#2785,.T.);
#3788=ORIENTED_EDGE('',*,*,#2792,.T.);
#3789=ORIENTED_EDGE('',*,*,#2793,.F.);
#3790=ORIENTED_EDGE('',*,*,#2772,.F.);
#3791=ORIENTED_EDGE('',*,*,#2762,.T.);
#3792=ORIENTED_EDGE('',*,*,#2773,.T.);
#3793=ORIENTED_EDGE('',*,*,#2793,.T.);
#3794=ORIENTED_EDGE('',*,*,#2791,.T.);
#3795=ORIENTED_EDGE('',*,*,#2774,.T.);
#3796=ORIENTED_EDGE('',*,*,#2794,.F.);
#3797=ORIENTED_EDGE('',*,*,#2795,.F.);
#3798=ORIENTED_EDGE('',*,*,#2796,.F.);
#3799=ORIENTED_EDGE('',*,*,#2797,.T.);
#3800=ORIENTED_EDGE('',*,*,#2794,.T.);
#3801=ORIENTED_EDGE('',*,*,#2797,.F.);
#3802=ORIENTED_EDGE('',*,*,#2798,.T.);
#3803=ORIENTED_EDGE('',*,*,#2799,.F.);
#3804=ORIENTED_EDGE('',*,*,#2798,.F.);
#3805=ORIENTED_EDGE('',*,*,#2800,.T.);
#3806=ORIENTED_EDGE('',*,*,#2801,.T.);
#3807=ORIENTED_EDGE('',*,*,#2800,.F.);
#3808=ORIENTED_EDGE('',*,*,#2801,.F.);
#3809=ORIENTED_EDGE('',*,*,#2795,.T.);
#3810=ORIENTED_EDGE('',*,*,#2802,.T.);
#3811=ORIENTED_EDGE('',*,*,#2799,.T.);
#3812=ORIENTED_EDGE('',*,*,#2802,.F.);
#3813=ORIENTED_EDGE('',*,*,#2796,.T.);
#3814=ORIENTED_EDGE('',*,*,#2803,.F.);
#3815=ORIENTED_EDGE('',*,*,#2804,.T.);
#3816=ORIENTED_EDGE('',*,*,#2805,.T.);
#3817=ORIENTED_EDGE('',*,*,#2806,.T.);
#3818=ORIENTED_EDGE('',*,*,#2807,.F.);
#3819=ORIENTED_EDGE('',*,*,#2808,.T.);
#3820=ORIENTED_EDGE('',*,*,#2803,.T.);
#3821=ORIENTED_EDGE('',*,*,#2809,.T.);
#3822=ORIENTED_EDGE('',*,*,#2810,.F.);
#3823=ORIENTED_EDGE('',*,*,#2811,.T.);
#3824=ORIENTED_EDGE('',*,*,#2807,.T.);
#3825=ORIENTED_EDGE('',*,*,#2812,.T.);
#3826=ORIENTED_EDGE('',*,*,#2813,.F.);
#3827=ORIENTED_EDGE('',*,*,#2814,.T.);
#3828=ORIENTED_EDGE('',*,*,#2810,.T.);
#3829=ORIENTED_EDGE('',*,*,#2815,.T.);
#3830=ORIENTED_EDGE('',*,*,#2816,.F.);
#3831=ORIENTED_EDGE('',*,*,#2817,.T.);
#3832=ORIENTED_EDGE('',*,*,#2813,.T.);
#3833=ORIENTED_EDGE('',*,*,#2818,.T.);
#3834=ORIENTED_EDGE('',*,*,#2819,.F.);
#3835=ORIENTED_EDGE('',*,*,#2820,.T.);
#3836=ORIENTED_EDGE('',*,*,#2816,.T.);
#3837=ORIENTED_EDGE('',*,*,#2821,.T.);
#3838=ORIENTED_EDGE('',*,*,#2822,.F.);
#3839=ORIENTED_EDGE('',*,*,#2823,.T.);
#3840=ORIENTED_EDGE('',*,*,#2819,.T.);
#3841=ORIENTED_EDGE('',*,*,#2824,.T.);
#3842=ORIENTED_EDGE('',*,*,#2825,.F.);
#3843=ORIENTED_EDGE('',*,*,#2826,.T.);
#3844=ORIENTED_EDGE('',*,*,#2822,.T.);
#3845=ORIENTED_EDGE('',*,*,#2827,.T.);
#3846=ORIENTED_EDGE('',*,*,#2828,.F.);
#3847=ORIENTED_EDGE('',*,*,#2829,.T.);
#3848=ORIENTED_EDGE('',*,*,#2825,.T.);
#3849=ORIENTED_EDGE('',*,*,#2830,.T.);
#3850=ORIENTED_EDGE('',*,*,#2831,.F.);
#3851=ORIENTED_EDGE('',*,*,#2832,.T.);
#3852=ORIENTED_EDGE('',*,*,#2828,.T.);
#3853=ORIENTED_EDGE('',*,*,#2833,.T.);
#3854=ORIENTED_EDGE('',*,*,#2834,.F.);
#3855=ORIENTED_EDGE('',*,*,#2835,.T.);
#3856=ORIENTED_EDGE('',*,*,#2831,.T.);
#3857=ORIENTED_EDGE('',*,*,#2836,.T.);
#3858=ORIENTED_EDGE('',*,*,#2837,.F.);
#3859=ORIENTED_EDGE('',*,*,#2838,.T.);
#3860=ORIENTED_EDGE('',*,*,#2834,.T.);
#3861=ORIENTED_EDGE('',*,*,#2839,.T.);
#3862=ORIENTED_EDGE('',*,*,#2840,.F.);
#3863=ORIENTED_EDGE('',*,*,#2841,.T.);
#3864=ORIENTED_EDGE('',*,*,#2837,.T.);
#3865=ORIENTED_EDGE('',*,*,#2842,.T.);
#3866=ORIENTED_EDGE('',*,*,#2843,.F.);
#3867=ORIENTED_EDGE('',*,*,#2844,.T.);
#3868=ORIENTED_EDGE('',*,*,#2840,.T.);
#3869=ORIENTED_EDGE('',*,*,#2845,.T.);
#3870=ORIENTED_EDGE('',*,*,#2846,.F.);
#3871=ORIENTED_EDGE('',*,*,#2847,.T.);
#3872=ORIENTED_EDGE('',*,*,#2843,.T.);
#3873=ORIENTED_EDGE('',*,*,#2848,.T.);
#3874=ORIENTED_EDGE('',*,*,#2849,.F.);
#3875=ORIENTED_EDGE('',*,*,#2850,.T.);
#3876=ORIENTED_EDGE('',*,*,#2846,.T.);
#3877=ORIENTED_EDGE('',*,*,#2851,.T.);
#3878=ORIENTED_EDGE('',*,*,#2852,.F.);
#3879=ORIENTED_EDGE('',*,*,#2853,.T.);
#3880=ORIENTED_EDGE('',*,*,#2849,.T.);
#3881=ORIENTED_EDGE('',*,*,#2854,.T.);
#3882=ORIENTED_EDGE('',*,*,#2855,.F.);
#3883=ORIENTED_EDGE('',*,*,#2856,.T.);
#3884=ORIENTED_EDGE('',*,*,#2852,.T.);
#3885=ORIENTED_EDGE('',*,*,#2857,.T.);
#3886=ORIENTED_EDGE('',*,*,#2858,.F.);
#3887=ORIENTED_EDGE('',*,*,#2859,.T.);
#3888=ORIENTED_EDGE('',*,*,#2855,.T.);
#3889=ORIENTED_EDGE('',*,*,#2860,.T.);
#3890=ORIENTED_EDGE('',*,*,#2861,.F.);
#3891=ORIENTED_EDGE('',*,*,#2862,.T.);
#3892=ORIENTED_EDGE('',*,*,#2858,.T.);
#3893=ORIENTED_EDGE('',*,*,#2863,.T.);
#3894=ORIENTED_EDGE('',*,*,#2864,.F.);
#3895=ORIENTED_EDGE('',*,*,#2865,.T.);
#3896=ORIENTED_EDGE('',*,*,#2861,.T.);
#3897=ORIENTED_EDGE('',*,*,#2866,.T.);
#3898=ORIENTED_EDGE('',*,*,#2867,.F.);
#3899=ORIENTED_EDGE('',*,*,#2868,.T.);
#3900=ORIENTED_EDGE('',*,*,#2864,.T.);
#3901=ORIENTED_EDGE('',*,*,#2869,.T.);
#3902=ORIENTED_EDGE('',*,*,#2870,.F.);
#3903=ORIENTED_EDGE('',*,*,#2871,.T.);
#3904=ORIENTED_EDGE('',*,*,#2867,.T.);
#3905=ORIENTED_EDGE('',*,*,#2872,.T.);
#3906=ORIENTED_EDGE('',*,*,#2873,.F.);
#3907=ORIENTED_EDGE('',*,*,#2874,.T.);
#3908=ORIENTED_EDGE('',*,*,#2870,.T.);
#3909=ORIENTED_EDGE('',*,*,#2875,.T.);
#3910=ORIENTED_EDGE('',*,*,#2876,.F.);
#3911=ORIENTED_EDGE('',*,*,#2877,.T.);
#3912=ORIENTED_EDGE('',*,*,#2873,.T.);
#3913=ORIENTED_EDGE('',*,*,#2878,.T.);
#3914=ORIENTED_EDGE('',*,*,#2879,.F.);
#3915=ORIENTED_EDGE('',*,*,#2880,.T.);
#3916=ORIENTED_EDGE('',*,*,#2876,.T.);
#3917=ORIENTED_EDGE('',*,*,#2881,.T.);
#3918=ORIENTED_EDGE('',*,*,#2882,.F.);
#3919=ORIENTED_EDGE('',*,*,#2883,.T.);
#3920=ORIENTED_EDGE('',*,*,#2879,.T.);
#3921=ORIENTED_EDGE('',*,*,#2884,.T.);
#3922=ORIENTED_EDGE('',*,*,#2885,.F.);
#3923=ORIENTED_EDGE('',*,*,#2886,.T.);
#3924=ORIENTED_EDGE('',*,*,#2882,.T.);
#3925=ORIENTED_EDGE('',*,*,#2887,.T.);
#3926=ORIENTED_EDGE('',*,*,#2888,.F.);
#3927=ORIENTED_EDGE('',*,*,#2889,.T.);
#3928=ORIENTED_EDGE('',*,*,#2885,.T.);
#3929=ORIENTED_EDGE('',*,*,#2890,.T.);
#3930=ORIENTED_EDGE('',*,*,#2891,.F.);
#3931=ORIENTED_EDGE('',*,*,#2892,.T.);
#3932=ORIENTED_EDGE('',*,*,#2888,.T.);
#3933=ORIENTED_EDGE('',*,*,#2893,.T.);
#3934=ORIENTED_EDGE('',*,*,#2894,.F.);
#3935=ORIENTED_EDGE('',*,*,#2895,.T.);
#3936=ORIENTED_EDGE('',*,*,#2891,.T.);
#3937=ORIENTED_EDGE('',*,*,#2896,.T.);
#3938=ORIENTED_EDGE('',*,*,#2897,.F.);
#3939=ORIENTED_EDGE('',*,*,#2898,.T.);
#3940=ORIENTED_EDGE('',*,*,#2894,.T.);
#3941=ORIENTED_EDGE('',*,*,#2899,.T.);
#3942=ORIENTED_EDGE('',*,*,#2900,.F.);
#3943=ORIENTED_EDGE('',*,*,#2901,.T.);
#3944=ORIENTED_EDGE('',*,*,#2897,.T.);
#3945=ORIENTED_EDGE('',*,*,#2902,.T.);
#3946=ORIENTED_EDGE('',*,*,#2903,.F.);
#3947=ORIENTED_EDGE('',*,*,#2904,.T.);
#3948=ORIENTED_EDGE('',*,*,#2900,.T.);
#3949=ORIENTED_EDGE('',*,*,#2905,.T.);
#3950=ORIENTED_EDGE('',*,*,#2906,.F.);
#3951=ORIENTED_EDGE('',*,*,#2907,.F.);
#3952=ORIENTED_EDGE('',*,*,#2908,.T.);
#3953=ORIENTED_EDGE('',*,*,#2903,.T.);
#3954=ORIENTED_EDGE('',*,*,#2909,.T.);
#3955=ORIENTED_EDGE('',*,*,#2910,.F.);
#3956=ORIENTED_EDGE('',*,*,#2911,.T.);
#3957=ORIENTED_EDGE('',*,*,#2912,.F.);
#3958=ORIENTED_EDGE('',*,*,#2913,.F.);
#3959=ORIENTED_EDGE('',*,*,#2914,.F.);
#3960=ORIENTED_EDGE('',*,*,#2915,.T.);
#3961=ORIENTED_EDGE('',*,*,#2910,.T.);
#3962=ORIENTED_EDGE('',*,*,#2916,.F.);
#3963=ORIENTED_EDGE('',*,*,#2917,.F.);
#3964=ORIENTED_EDGE('',*,*,#2918,.T.);
#3965=ORIENTED_EDGE('',*,*,#2914,.T.);
#3966=ORIENTED_EDGE('',*,*,#2919,.F.);
#3967=ORIENTED_EDGE('',*,*,#2920,.F.);
#3968=ORIENTED_EDGE('',*,*,#2921,.T.);
#3969=ORIENTED_EDGE('',*,*,#2917,.T.);
#3970=ORIENTED_EDGE('',*,*,#2922,.F.);
#3971=ORIENTED_EDGE('',*,*,#2923,.F.);
#3972=ORIENTED_EDGE('',*,*,#2924,.T.);
#3973=ORIENTED_EDGE('',*,*,#2920,.T.);
#3974=ORIENTED_EDGE('',*,*,#2925,.F.);
#3975=ORIENTED_EDGE('',*,*,#2926,.F.);
#3976=ORIENTED_EDGE('',*,*,#2927,.T.);
#3977=ORIENTED_EDGE('',*,*,#2923,.T.);
#3978=ORIENTED_EDGE('',*,*,#2928,.F.);
#3979=ORIENTED_EDGE('',*,*,#2929,.F.);
#3980=ORIENTED_EDGE('',*,*,#2930,.T.);
#3981=ORIENTED_EDGE('',*,*,#2926,.T.);
#3982=ORIENTED_EDGE('',*,*,#2931,.F.);
#3983=ORIENTED_EDGE('',*,*,#2932,.F.);
#3984=ORIENTED_EDGE('',*,*,#2933,.T.);
#3985=ORIENTED_EDGE('',*,*,#2929,.T.);
#3986=ORIENTED_EDGE('',*,*,#2934,.F.);
#3987=ORIENTED_EDGE('',*,*,#2935,.F.);
#3988=ORIENTED_EDGE('',*,*,#2936,.T.);
#3989=ORIENTED_EDGE('',*,*,#2932,.T.);
#3990=ORIENTED_EDGE('',*,*,#2937,.F.);
#3991=ORIENTED_EDGE('',*,*,#2938,.F.);
#3992=ORIENTED_EDGE('',*,*,#2939,.T.);
#3993=ORIENTED_EDGE('',*,*,#2935,.T.);
#3994=ORIENTED_EDGE('',*,*,#2940,.F.);
#3995=ORIENTED_EDGE('',*,*,#2941,.F.);
#3996=ORIENTED_EDGE('',*,*,#2942,.T.);
#3997=ORIENTED_EDGE('',*,*,#2938,.T.);
#3998=ORIENTED_EDGE('',*,*,#2943,.F.);
#3999=ORIENTED_EDGE('',*,*,#2944,.F.);
#4000=ORIENTED_EDGE('',*,*,#2945,.T.);
#4001=ORIENTED_EDGE('',*,*,#2941,.T.);
#4002=ORIENTED_EDGE('',*,*,#2946,.F.);
#4003=ORIENTED_EDGE('',*,*,#2947,.F.);
#4004=ORIENTED_EDGE('',*,*,#2948,.T.);
#4005=ORIENTED_EDGE('',*,*,#2944,.T.);
#4006=ORIENTED_EDGE('',*,*,#2949,.F.);
#4007=ORIENTED_EDGE('',*,*,#2950,.F.);
#4008=ORIENTED_EDGE('',*,*,#2951,.T.);
#4009=ORIENTED_EDGE('',*,*,#2947,.T.);
#4010=ORIENTED_EDGE('',*,*,#2952,.F.);
#4011=ORIENTED_EDGE('',*,*,#2953,.F.);
#4012=ORIENTED_EDGE('',*,*,#2954,.T.);
#4013=ORIENTED_EDGE('',*,*,#2950,.T.);
#4014=ORIENTED_EDGE('',*,*,#2955,.F.);
#4015=ORIENTED_EDGE('',*,*,#2956,.F.);
#4016=ORIENTED_EDGE('',*,*,#2957,.T.);
#4017=ORIENTED_EDGE('',*,*,#2953,.T.);
#4018=ORIENTED_EDGE('',*,*,#2958,.F.);
#4019=ORIENTED_EDGE('',*,*,#2959,.F.);
#4020=ORIENTED_EDGE('',*,*,#2960,.T.);
#4021=ORIENTED_EDGE('',*,*,#2956,.T.);
#4022=ORIENTED_EDGE('',*,*,#2961,.F.);
#4023=ORIENTED_EDGE('',*,*,#2962,.F.);
#4024=ORIENTED_EDGE('',*,*,#2963,.T.);
#4025=ORIENTED_EDGE('',*,*,#2959,.T.);
#4026=ORIENTED_EDGE('',*,*,#2964,.F.);
#4027=ORIENTED_EDGE('',*,*,#2965,.F.);
#4028=ORIENTED_EDGE('',*,*,#2966,.T.);
#4029=ORIENTED_EDGE('',*,*,#2962,.T.);
#4030=ORIENTED_EDGE('',*,*,#2967,.F.);
#4031=ORIENTED_EDGE('',*,*,#2968,.F.);
#4032=ORIENTED_EDGE('',*,*,#2969,.T.);
#4033=ORIENTED_EDGE('',*,*,#2965,.T.);
#4034=ORIENTED_EDGE('',*,*,#2970,.F.);
#4035=ORIENTED_EDGE('',*,*,#2971,.F.);
#4036=ORIENTED_EDGE('',*,*,#2972,.T.);
#4037=ORIENTED_EDGE('',*,*,#2968,.T.);
#4038=ORIENTED_EDGE('',*,*,#2973,.F.);
#4039=ORIENTED_EDGE('',*,*,#2974,.F.);
#4040=ORIENTED_EDGE('',*,*,#2975,.T.);
#4041=ORIENTED_EDGE('',*,*,#2971,.T.);
#4042=ORIENTED_EDGE('',*,*,#2976,.F.);
#4043=ORIENTED_EDGE('',*,*,#2977,.F.);
#4044=ORIENTED_EDGE('',*,*,#2978,.T.);
#4045=ORIENTED_EDGE('',*,*,#2974,.T.);
#4046=ORIENTED_EDGE('',*,*,#2979,.F.);
#4047=ORIENTED_EDGE('',*,*,#2980,.F.);
#4048=ORIENTED_EDGE('',*,*,#2981,.T.);
#4049=ORIENTED_EDGE('',*,*,#2977,.T.);
#4050=ORIENTED_EDGE('',*,*,#2982,.F.);
#4051=ORIENTED_EDGE('',*,*,#2983,.F.);
#4052=ORIENTED_EDGE('',*,*,#2984,.T.);
#4053=ORIENTED_EDGE('',*,*,#2980,.T.);
#4054=ORIENTED_EDGE('',*,*,#2985,.F.);
#4055=ORIENTED_EDGE('',*,*,#2986,.F.);
#4056=ORIENTED_EDGE('',*,*,#2987,.T.);
#4057=ORIENTED_EDGE('',*,*,#2983,.T.);
#4058=ORIENTED_EDGE('',*,*,#2988,.F.);
#4059=ORIENTED_EDGE('',*,*,#2989,.F.);
#4060=ORIENTED_EDGE('',*,*,#2990,.T.);
#4061=ORIENTED_EDGE('',*,*,#2986,.T.);
#4062=ORIENTED_EDGE('',*,*,#2991,.F.);
#4063=ORIENTED_EDGE('',*,*,#2992,.F.);
#4064=ORIENTED_EDGE('',*,*,#2993,.T.);
#4065=ORIENTED_EDGE('',*,*,#2989,.T.);
#4066=ORIENTED_EDGE('',*,*,#2994,.F.);
#4067=ORIENTED_EDGE('',*,*,#2995,.F.);
#4068=ORIENTED_EDGE('',*,*,#2996,.T.);
#4069=ORIENTED_EDGE('',*,*,#2992,.T.);
#4070=ORIENTED_EDGE('',*,*,#2997,.F.);
#4071=ORIENTED_EDGE('',*,*,#2998,.F.);
#4072=ORIENTED_EDGE('',*,*,#2999,.T.);
#4073=ORIENTED_EDGE('',*,*,#2995,.T.);
#4074=ORIENTED_EDGE('',*,*,#3000,.F.);
#4075=ORIENTED_EDGE('',*,*,#3001,.F.);
#4076=ORIENTED_EDGE('',*,*,#3002,.T.);
#4077=ORIENTED_EDGE('',*,*,#2998,.T.);
#4078=ORIENTED_EDGE('',*,*,#3003,.F.);
#4079=ORIENTED_EDGE('',*,*,#3004,.F.);
#4080=ORIENTED_EDGE('',*,*,#3005,.T.);
#4081=ORIENTED_EDGE('',*,*,#3001,.T.);
#4082=ORIENTED_EDGE('',*,*,#3006,.F.);
#4083=ORIENTED_EDGE('',*,*,#3007,.F.);
#4084=ORIENTED_EDGE('',*,*,#3008,.T.);
#4085=ORIENTED_EDGE('',*,*,#3004,.T.);
#4086=ORIENTED_EDGE('',*,*,#3009,.F.);
#4087=ORIENTED_EDGE('',*,*,#3010,.F.);
#4088=ORIENTED_EDGE('',*,*,#3011,.T.);
#4089=ORIENTED_EDGE('',*,*,#3007,.T.);
#4090=ORIENTED_EDGE('',*,*,#3012,.F.);
#4091=ORIENTED_EDGE('',*,*,#3013,.F.);
#4092=ORIENTED_EDGE('',*,*,#3014,.F.);
#4093=ORIENTED_EDGE('',*,*,#2909,.F.);
#4094=ORIENTED_EDGE('',*,*,#2905,.F.);
#4095=ORIENTED_EDGE('',*,*,#2902,.F.);
#4096=ORIENTED_EDGE('',*,*,#2899,.F.);
#4097=ORIENTED_EDGE('',*,*,#2896,.F.);
#4098=ORIENTED_EDGE('',*,*,#2893,.F.);
#4099=ORIENTED_EDGE('',*,*,#2890,.F.);
#4100=ORIENTED_EDGE('',*,*,#2887,.F.);
#4101=ORIENTED_EDGE('',*,*,#2884,.F.);
#4102=ORIENTED_EDGE('',*,*,#2881,.F.);
#4103=ORIENTED_EDGE('',*,*,#2878,.F.);
#4104=ORIENTED_EDGE('',*,*,#2875,.F.);
#4105=ORIENTED_EDGE('',*,*,#2872,.F.);
#4106=ORIENTED_EDGE('',*,*,#2869,.F.);
#4107=ORIENTED_EDGE('',*,*,#2866,.F.);
#4108=ORIENTED_EDGE('',*,*,#2863,.F.);
#4109=ORIENTED_EDGE('',*,*,#2860,.F.);
#4110=ORIENTED_EDGE('',*,*,#2857,.F.);
#4111=ORIENTED_EDGE('',*,*,#2854,.F.);
#4112=ORIENTED_EDGE('',*,*,#2851,.F.);
#4113=ORIENTED_EDGE('',*,*,#2848,.F.);
#4114=ORIENTED_EDGE('',*,*,#2845,.F.);
#4115=ORIENTED_EDGE('',*,*,#2842,.F.);
#4116=ORIENTED_EDGE('',*,*,#2839,.F.);
#4117=ORIENTED_EDGE('',*,*,#2836,.F.);
#4118=ORIENTED_EDGE('',*,*,#2833,.F.);
#4119=ORIENTED_EDGE('',*,*,#2830,.F.);
#4120=ORIENTED_EDGE('',*,*,#2827,.F.);
#4121=ORIENTED_EDGE('',*,*,#2824,.F.);
#4122=ORIENTED_EDGE('',*,*,#2821,.F.);
#4123=ORIENTED_EDGE('',*,*,#2818,.F.);
#4124=ORIENTED_EDGE('',*,*,#2815,.F.);
#4125=ORIENTED_EDGE('',*,*,#2812,.F.);
#4126=ORIENTED_EDGE('',*,*,#2809,.F.);
#4127=ORIENTED_EDGE('',*,*,#2806,.F.);
#4128=ORIENTED_EDGE('',*,*,#3015,.F.);
#4129=ORIENTED_EDGE('',*,*,#3016,.T.);
#4130=ORIENTED_EDGE('',*,*,#3012,.T.);
#4131=ORIENTED_EDGE('',*,*,#3009,.T.);
#4132=ORIENTED_EDGE('',*,*,#3006,.T.);
#4133=ORIENTED_EDGE('',*,*,#3003,.T.);
#4134=ORIENTED_EDGE('',*,*,#3000,.T.);
#4135=ORIENTED_EDGE('',*,*,#2997,.T.);
#4136=ORIENTED_EDGE('',*,*,#2994,.T.);
#4137=ORIENTED_EDGE('',*,*,#2991,.T.);
#4138=ORIENTED_EDGE('',*,*,#2988,.T.);
#4139=ORIENTED_EDGE('',*,*,#2985,.T.);
#4140=ORIENTED_EDGE('',*,*,#2982,.T.);
#4141=ORIENTED_EDGE('',*,*,#2979,.T.);
#4142=ORIENTED_EDGE('',*,*,#2976,.T.);
#4143=ORIENTED_EDGE('',*,*,#2973,.T.);
#4144=ORIENTED_EDGE('',*,*,#2970,.T.);
#4145=ORIENTED_EDGE('',*,*,#2967,.T.);
#4146=ORIENTED_EDGE('',*,*,#2964,.T.);
#4147=ORIENTED_EDGE('',*,*,#2961,.T.);
#4148=ORIENTED_EDGE('',*,*,#2958,.T.);
#4149=ORIENTED_EDGE('',*,*,#2955,.T.);
#4150=ORIENTED_EDGE('',*,*,#2952,.T.);
#4151=ORIENTED_EDGE('',*,*,#2949,.T.);
#4152=ORIENTED_EDGE('',*,*,#2946,.T.);
#4153=ORIENTED_EDGE('',*,*,#2943,.T.);
#4154=ORIENTED_EDGE('',*,*,#2940,.T.);
#4155=ORIENTED_EDGE('',*,*,#2937,.T.);
#4156=ORIENTED_EDGE('',*,*,#2934,.T.);
#4157=ORIENTED_EDGE('',*,*,#2931,.T.);
#4158=ORIENTED_EDGE('',*,*,#2928,.T.);
#4159=ORIENTED_EDGE('',*,*,#2925,.T.);
#4160=ORIENTED_EDGE('',*,*,#2922,.T.);
#4161=ORIENTED_EDGE('',*,*,#2919,.T.);
#4162=ORIENTED_EDGE('',*,*,#2916,.T.);
#4163=ORIENTED_EDGE('',*,*,#2913,.T.);
#4164=ORIENTED_EDGE('',*,*,#3010,.T.);
#4165=ORIENTED_EDGE('',*,*,#3016,.F.);
#4166=ORIENTED_EDGE('',*,*,#3017,.F.);
#4167=ORIENTED_EDGE('',*,*,#3018,.T.);
#4168=ORIENTED_EDGE('',*,*,#3019,.F.);
#4169=ORIENTED_EDGE('',*,*,#2911,.F.);
#4170=ORIENTED_EDGE('',*,*,#2915,.F.);
#4171=ORIENTED_EDGE('',*,*,#2918,.F.);
#4172=ORIENTED_EDGE('',*,*,#2921,.F.);
#4173=ORIENTED_EDGE('',*,*,#2924,.F.);
#4174=ORIENTED_EDGE('',*,*,#2927,.F.);
#4175=ORIENTED_EDGE('',*,*,#2930,.F.);
#4176=ORIENTED_EDGE('',*,*,#2933,.F.);
#4177=ORIENTED_EDGE('',*,*,#2936,.F.);
#4178=ORIENTED_EDGE('',*,*,#2939,.F.);
#4179=ORIENTED_EDGE('',*,*,#2942,.F.);
#4180=ORIENTED_EDGE('',*,*,#2945,.F.);
#4181=ORIENTED_EDGE('',*,*,#2948,.F.);
#4182=ORIENTED_EDGE('',*,*,#2951,.F.);
#4183=ORIENTED_EDGE('',*,*,#2954,.F.);
#4184=ORIENTED_EDGE('',*,*,#2957,.F.);
#4185=ORIENTED_EDGE('',*,*,#2960,.F.);
#4186=ORIENTED_EDGE('',*,*,#2963,.F.);
#4187=ORIENTED_EDGE('',*,*,#2966,.F.);
#4188=ORIENTED_EDGE('',*,*,#2969,.F.);
#4189=ORIENTED_EDGE('',*,*,#2972,.F.);
#4190=ORIENTED_EDGE('',*,*,#2975,.F.);
#4191=ORIENTED_EDGE('',*,*,#2978,.F.);
#4192=ORIENTED_EDGE('',*,*,#2981,.F.);
#4193=ORIENTED_EDGE('',*,*,#2984,.F.);
#4194=ORIENTED_EDGE('',*,*,#2987,.F.);
#4195=ORIENTED_EDGE('',*,*,#2990,.F.);
#4196=ORIENTED_EDGE('',*,*,#2993,.F.);
#4197=ORIENTED_EDGE('',*,*,#2996,.F.);
#4198=ORIENTED_EDGE('',*,*,#2999,.F.);
#4199=ORIENTED_EDGE('',*,*,#3002,.F.);
#4200=ORIENTED_EDGE('',*,*,#3005,.F.);
#4201=ORIENTED_EDGE('',*,*,#3008,.F.);
#4202=ORIENTED_EDGE('',*,*,#3011,.F.);
#4203=ORIENTED_EDGE('',*,*,#3018,.F.);
#4204=ORIENTED_EDGE('',*,*,#3020,.F.);
#4205=ORIENTED_EDGE('',*,*,#2804,.F.);
#4206=ORIENTED_EDGE('',*,*,#2808,.F.);
#4207=ORIENTED_EDGE('',*,*,#2811,.F.);
#4208=ORIENTED_EDGE('',*,*,#2814,.F.);
#4209=ORIENTED_EDGE('',*,*,#2817,.F.);
#4210=ORIENTED_EDGE('',*,*,#2820,.F.);
#4211=ORIENTED_EDGE('',*,*,#2823,.F.);
#4212=ORIENTED_EDGE('',*,*,#2826,.F.);
#4213=ORIENTED_EDGE('',*,*,#2829,.F.);
#4214=ORIENTED_EDGE('',*,*,#2832,.F.);
#4215=ORIENTED_EDGE('',*,*,#2835,.F.);
#4216=ORIENTED_EDGE('',*,*,#2838,.F.);
#4217=ORIENTED_EDGE('',*,*,#2841,.F.);
#4218=ORIENTED_EDGE('',*,*,#2844,.F.);
#4219=ORIENTED_EDGE('',*,*,#2847,.F.);
#4220=ORIENTED_EDGE('',*,*,#2850,.F.);
#4221=ORIENTED_EDGE('',*,*,#2853,.F.);
#4222=ORIENTED_EDGE('',*,*,#2856,.F.);
#4223=ORIENTED_EDGE('',*,*,#2859,.F.);
#4224=ORIENTED_EDGE('',*,*,#2862,.F.);
#4225=ORIENTED_EDGE('',*,*,#2865,.F.);
#4226=ORIENTED_EDGE('',*,*,#2868,.F.);
#4227=ORIENTED_EDGE('',*,*,#2871,.F.);
#4228=ORIENTED_EDGE('',*,*,#2874,.F.);
#4229=ORIENTED_EDGE('',*,*,#2877,.F.);
#4230=ORIENTED_EDGE('',*,*,#2880,.F.);
#4231=ORIENTED_EDGE('',*,*,#2883,.F.);
#4232=ORIENTED_EDGE('',*,*,#2886,.F.);
#4233=ORIENTED_EDGE('',*,*,#2889,.F.);
#4234=ORIENTED_EDGE('',*,*,#2892,.F.);
#4235=ORIENTED_EDGE('',*,*,#2895,.F.);
#4236=ORIENTED_EDGE('',*,*,#2898,.F.);
#4237=ORIENTED_EDGE('',*,*,#2901,.F.);
#4238=ORIENTED_EDGE('',*,*,#2904,.F.);
#4239=ORIENTED_EDGE('',*,*,#2908,.F.);
#4240=ORIENTED_EDGE('',*,*,#2906,.T.);
#4241=ORIENTED_EDGE('',*,*,#3014,.T.);
#4242=ORIENTED_EDGE('',*,*,#3021,.F.);
#4243=ORIENTED_EDGE('',*,*,#3022,.F.);
#4244=ORIENTED_EDGE('',*,*,#3023,.T.);
#4245=ORIENTED_EDGE('',*,*,#3024,.T.);
#4246=ORIENTED_EDGE('',*,*,#3025,.F.);
#4247=ORIENTED_EDGE('',*,*,#3026,.F.);
#4248=ORIENTED_EDGE('',*,*,#3027,.T.);
#4249=ORIENTED_EDGE('',*,*,#3028,.T.);
#4250=ORIENTED_EDGE('',*,*,#3023,.F.);
#4251=ORIENTED_EDGE('',*,*,#3029,.F.);
#4252=ORIENTED_EDGE('',*,*,#3030,.T.);
#4253=ORIENTED_EDGE('',*,*,#3031,.T.);
#4254=ORIENTED_EDGE('',*,*,#3027,.F.);
#4255=ORIENTED_EDGE('',*,*,#3032,.F.);
#4256=ORIENTED_EDGE('',*,*,#3033,.T.);
#4257=ORIENTED_EDGE('',*,*,#3034,.T.);
#4258=ORIENTED_EDGE('',*,*,#3030,.F.);
#4259=ORIENTED_EDGE('',*,*,#3035,.F.);
#4260=ORIENTED_EDGE('',*,*,#3036,.T.);
#4261=ORIENTED_EDGE('',*,*,#3037,.T.);
#4262=ORIENTED_EDGE('',*,*,#3033,.F.);
#4263=ORIENTED_EDGE('',*,*,#3038,.F.);
#4264=ORIENTED_EDGE('',*,*,#3025,.T.);
#4265=ORIENTED_EDGE('',*,*,#3039,.T.);
#4266=ORIENTED_EDGE('',*,*,#3036,.F.);
#4267=ORIENTED_EDGE('',*,*,#3039,.F.);
#4268=ORIENTED_EDGE('',*,*,#3024,.F.);
#4269=ORIENTED_EDGE('',*,*,#3028,.F.);
#4270=ORIENTED_EDGE('',*,*,#3031,.F.);
#4271=ORIENTED_EDGE('',*,*,#3034,.F.);
#4272=ORIENTED_EDGE('',*,*,#3037,.F.);
#4273=ORIENTED_EDGE('',*,*,#3040,.T.);
#4274=ORIENTED_EDGE('',*,*,#3020,.T.);
#4275=ORIENTED_EDGE('',*,*,#3017,.T.);
#4276=ORIENTED_EDGE('',*,*,#3015,.T.);
#4277=ORIENTED_EDGE('',*,*,#2805,.F.);
#4278=ORIENTED_EDGE('',*,*,#3040,.F.);
#4279=ORIENTED_EDGE('',*,*,#3041,.T.);
#4280=ORIENTED_EDGE('',*,*,#3042,.T.);
#4281=ORIENTED_EDGE('',*,*,#3041,.F.);
#4282=ORIENTED_EDGE('',*,*,#3042,.F.);
#4283=ORIENTED_EDGE('',*,*,#3022,.T.);
#4284=ORIENTED_EDGE('',*,*,#3038,.T.);
#4285=ORIENTED_EDGE('',*,*,#3035,.T.);
#4286=ORIENTED_EDGE('',*,*,#3032,.T.);
#4287=ORIENTED_EDGE('',*,*,#3029,.T.);
#4288=ORIENTED_EDGE('',*,*,#3026,.T.);
#4289=ORIENTED_EDGE('',*,*,#3019,.T.);
#4290=ORIENTED_EDGE('',*,*,#2907,.T.);
#4291=ORIENTED_EDGE('',*,*,#3021,.T.);
#4292=ORIENTED_EDGE('',*,*,#3013,.T.);
#4293=ORIENTED_EDGE('',*,*,#2912,.T.);
#4294=ORIENTED_EDGE('',*,*,#3043,.T.);
#4295=ORIENTED_EDGE('',*,*,#3044,.F.);
#4296=ORIENTED_EDGE('',*,*,#3045,.T.);
#4297=ORIENTED_EDGE('',*,*,#3046,.T.);
#4298=ORIENTED_EDGE('',*,*,#3047,.T.);
#4299=ORIENTED_EDGE('',*,*,#3048,.F.);
#4300=ORIENTED_EDGE('',*,*,#3043,.F.);
#4301=ORIENTED_EDGE('',*,*,#3049,.T.);
#4302=ORIENTED_EDGE('',*,*,#3050,.T.);
#4303=ORIENTED_EDGE('',*,*,#3051,.T.);
#4304=ORIENTED_EDGE('',*,*,#3046,.F.);
#4305=ORIENTED_EDGE('',*,*,#3052,.T.);
#4306=ORIENTED_EDGE('',*,*,#3053,.T.);
#4307=ORIENTED_EDGE('',*,*,#3054,.T.);
#4308=ORIENTED_EDGE('',*,*,#3050,.F.);
#4309=ORIENTED_EDGE('',*,*,#3055,.T.);
#4310=ORIENTED_EDGE('',*,*,#3056,.T.);
#4311=ORIENTED_EDGE('',*,*,#3057,.T.);
#4312=ORIENTED_EDGE('',*,*,#3053,.F.);
#4313=ORIENTED_EDGE('',*,*,#3058,.T.);
#4314=ORIENTED_EDGE('',*,*,#3059,.F.);
#4315=ORIENTED_EDGE('',*,*,#3060,.T.);
#4316=ORIENTED_EDGE('',*,*,#3061,.F.);
#4317=ORIENTED_EDGE('',*,*,#3062,.T.);
#4318=ORIENTED_EDGE('',*,*,#3063,.T.);
#4319=ORIENTED_EDGE('',*,*,#3064,.T.);
#4320=ORIENTED_EDGE('',*,*,#3065,.F.);
#4321=ORIENTED_EDGE('',*,*,#3066,.F.);
#4322=ORIENTED_EDGE('',*,*,#3067,.T.);
#4323=ORIENTED_EDGE('',*,*,#3068,.T.);
#4324=ORIENTED_EDGE('',*,*,#3063,.F.);
#4325=ORIENTED_EDGE('',*,*,#3069,.F.);
#4326=ORIENTED_EDGE('',*,*,#3070,.T.);
#4327=ORIENTED_EDGE('',*,*,#3071,.T.);
#4328=ORIENTED_EDGE('',*,*,#3067,.F.);
#4329=ORIENTED_EDGE('',*,*,#3072,.F.);
#4330=ORIENTED_EDGE('',*,*,#3073,.T.);
#4331=ORIENTED_EDGE('',*,*,#3074,.T.);
#4332=ORIENTED_EDGE('',*,*,#3070,.F.);
#4333=ORIENTED_EDGE('',*,*,#3075,.F.);
#4334=ORIENTED_EDGE('',*,*,#3076,.T.);
#4335=ORIENTED_EDGE('',*,*,#3077,.T.);
#4336=ORIENTED_EDGE('',*,*,#3073,.F.);
#4337=ORIENTED_EDGE('',*,*,#3078,.F.);
#4338=ORIENTED_EDGE('',*,*,#3079,.F.);
#4339=ORIENTED_EDGE('',*,*,#3080,.F.);
#4340=ORIENTED_EDGE('',*,*,#3081,.F.);
#4341=ORIENTED_EDGE('',*,*,#3082,.T.);
#4342=ORIENTED_EDGE('',*,*,#3079,.T.);
#4343=ORIENTED_EDGE('',*,*,#3083,.T.);
#4344=ORIENTED_EDGE('',*,*,#3076,.F.);
#4345=ORIENTED_EDGE('',*,*,#3084,.F.);
#4346=ORIENTED_EDGE('',*,*,#3085,.F.);
#4347=ORIENTED_EDGE('',*,*,#3064,.F.);
#4348=ORIENTED_EDGE('',*,*,#3068,.F.);
#4349=ORIENTED_EDGE('',*,*,#3071,.F.);
#4350=ORIENTED_EDGE('',*,*,#3074,.F.);
#4351=ORIENTED_EDGE('',*,*,#3077,.F.);
#4352=ORIENTED_EDGE('',*,*,#3083,.F.);
#4353=ORIENTED_EDGE('',*,*,#3082,.F.);
#4354=ORIENTED_EDGE('',*,*,#3086,.F.);
#4355=ORIENTED_EDGE('',*,*,#3060,.F.);
#4356=ORIENTED_EDGE('',*,*,#3087,.F.);
#4357=ORIENTED_EDGE('',*,*,#3058,.F.);
#4358=ORIENTED_EDGE('',*,*,#3055,.F.);
#4359=ORIENTED_EDGE('',*,*,#3052,.F.);
#4360=ORIENTED_EDGE('',*,*,#3049,.F.);
#4361=ORIENTED_EDGE('',*,*,#3045,.F.);
#4362=ORIENTED_EDGE('',*,*,#3088,.F.);
#4363=ORIENTED_EDGE('',*,*,#3047,.F.);
#4364=ORIENTED_EDGE('',*,*,#3051,.F.);
#4365=ORIENTED_EDGE('',*,*,#3054,.F.);
#4366=ORIENTED_EDGE('',*,*,#3057,.F.);
#4367=ORIENTED_EDGE('',*,*,#3089,.F.);
#4368=ORIENTED_EDGE('',*,*,#3062,.F.);
#4369=ORIENTED_EDGE('',*,*,#3090,.F.);
#4370=ORIENTED_EDGE('',*,*,#3080,.T.);
#4371=ORIENTED_EDGE('',*,*,#3084,.T.);
#4372=ORIENTED_EDGE('',*,*,#3078,.T.);
#4373=ORIENTED_EDGE('',*,*,#3075,.T.);
#4374=ORIENTED_EDGE('',*,*,#3072,.T.);
#4375=ORIENTED_EDGE('',*,*,#3069,.T.);
#4376=ORIENTED_EDGE('',*,*,#3066,.T.);
#4377=ORIENTED_EDGE('',*,*,#3091,.T.);
#4378=ORIENTED_EDGE('',*,*,#3092,.T.);
#4379=ORIENTED_EDGE('',*,*,#3093,.T.);
#4380=ORIENTED_EDGE('',*,*,#3094,.T.);
#4381=ORIENTED_EDGE('',*,*,#3095,.T.);
#4382=ORIENTED_EDGE('',*,*,#3096,.T.);
#4383=ORIENTED_EDGE('',*,*,#3086,.T.);
#4384=ORIENTED_EDGE('',*,*,#3081,.T.);
#4385=ORIENTED_EDGE('',*,*,#3090,.T.);
#4386=ORIENTED_EDGE('',*,*,#3061,.T.);
#4387=ORIENTED_EDGE('',*,*,#3059,.T.);
#4388=ORIENTED_EDGE('',*,*,#3089,.T.);
#4389=ORIENTED_EDGE('',*,*,#3056,.F.);
#4390=ORIENTED_EDGE('',*,*,#3087,.T.);
#4391=ORIENTED_EDGE('',*,*,#3097,.T.);
#4392=ORIENTED_EDGE('',*,*,#3098,.T.);
#4393=ORIENTED_EDGE('',*,*,#3096,.F.);
#4394=ORIENTED_EDGE('',*,*,#3099,.F.);
#4395=ORIENTED_EDGE('',*,*,#3100,.T.);
#4396=ORIENTED_EDGE('',*,*,#3099,.T.);
#4397=ORIENTED_EDGE('',*,*,#3095,.F.);
#4398=ORIENTED_EDGE('',*,*,#3101,.F.);
#4399=ORIENTED_EDGE('',*,*,#3102,.T.);
#4400=ORIENTED_EDGE('',*,*,#3101,.T.);
#4401=ORIENTED_EDGE('',*,*,#3094,.F.);
#4402=ORIENTED_EDGE('',*,*,#3103,.F.);
#4403=ORIENTED_EDGE('',*,*,#3104,.T.);
#4404=ORIENTED_EDGE('',*,*,#3103,.T.);
#4405=ORIENTED_EDGE('',*,*,#3093,.F.);
#4406=ORIENTED_EDGE('',*,*,#3105,.F.);
#4407=ORIENTED_EDGE('',*,*,#3106,.T.);
#4408=ORIENTED_EDGE('',*,*,#3105,.T.);
#4409=ORIENTED_EDGE('',*,*,#3092,.F.);
#4410=ORIENTED_EDGE('',*,*,#3107,.F.);
#4411=ORIENTED_EDGE('',*,*,#3108,.T.);
#4412=ORIENTED_EDGE('',*,*,#3107,.T.);
#4413=ORIENTED_EDGE('',*,*,#3091,.F.);
#4414=ORIENTED_EDGE('',*,*,#3098,.F.);
#4415=ORIENTED_EDGE('',*,*,#3108,.F.);
#4416=ORIENTED_EDGE('',*,*,#3097,.F.);
#4417=ORIENTED_EDGE('',*,*,#3100,.F.);
#4418=ORIENTED_EDGE('',*,*,#3102,.F.);
#4419=ORIENTED_EDGE('',*,*,#3104,.F.);
#4420=ORIENTED_EDGE('',*,*,#3106,.F.);
#4421=ORIENTED_EDGE('',*,*,#3085,.T.);
#4422=ORIENTED_EDGE('',*,*,#3044,.T.);
#4423=ORIENTED_EDGE('',*,*,#3048,.T.);
#4424=ORIENTED_EDGE('',*,*,#3088,.T.);
#4425=ORIENTED_EDGE('',*,*,#3065,.T.);
#4426=ORIENTED_EDGE('',*,*,#3109,.F.);
#4427=ORIENTED_EDGE('',*,*,#3110,.T.);
#4428=ORIENTED_EDGE('',*,*,#3111,.T.);
#4429=ORIENTED_EDGE('',*,*,#3110,.F.);
#4430=ORIENTED_EDGE('',*,*,#3109,.T.);
#4431=ORIENTED_EDGE('',*,*,#3111,.F.);
#4432=CYLINDRICAL_SURFACE('',#4956,0.5);
#4433=CYLINDRICAL_SURFACE('',#4961,0.5);
#4434=CYLINDRICAL_SURFACE('',#4966,0.409999999999997);
#4435=CYLINDRICAL_SURFACE('',#4970,0.409999999999997);
#4436=CYLINDRICAL_SURFACE('',#4974,0.409999999999997);
#4437=CYLINDRICAL_SURFACE('',#4978,0.409999999999997);
#4438=CYLINDRICAL_SURFACE('',#4982,0.225000000000001);
#4439=CYLINDRICAL_SURFACE('',#4984,0.224999999999994);
#4440=CYLINDRICAL_SURFACE('',#5009,0.409999999999997);
#4441=CYLINDRICAL_SURFACE('',#5013,0.409999999999997);
#4442=CYLINDRICAL_SURFACE('',#5017,0.409999999999997);
#4443=CYLINDRICAL_SURFACE('',#5021,0.409999999999997);
#4444=CYLINDRICAL_SURFACE('',#5025,0.225000000000001);
#4445=CYLINDRICAL_SURFACE('',#5028,0.224999999999994);
#4446=CYLINDRICAL_SURFACE('',#5082,1.);
#4447=CYLINDRICAL_SURFACE('',#5086,1.);
#4448=CYLINDRICAL_SURFACE('',#5089,0.225);
#4449=CYLINDRICAL_SURFACE('',#5092,0.225);
#4450=CYLINDRICAL_SURFACE('',#5102,0.225000000000001);
#4451=CYLINDRICAL_SURFACE('',#5105,0.224999999999994);
#4452=CYLINDRICAL_SURFACE('',#5110,0.42);
#4453=CYLINDRICAL_SURFACE('',#5119,0.4);
#4454=CYLINDRICAL_SURFACE('',#5121,0.22);
#4455=CYLINDRICAL_SURFACE('',#5125,0.22);
#4456=CYLINDRICAL_SURFACE('',#5128,0.4);
#4457=CYLINDRICAL_SURFACE('',#5135,0.225);
#4458=CYLINDRICAL_SURFACE('',#5138,0.225);
#4459=CYLINDRICAL_SURFACE('',#5143,0.42);
#4460=CYLINDRICAL_SURFACE('',#5147,0.42);
#4461=CYLINDRICAL_SURFACE('',#5155,0.22);
#4462=CYLINDRICAL_SURFACE('',#5157,0.4);
#4463=CYLINDRICAL_SURFACE('',#5167,0.3);
#4464=CYLINDRICAL_SURFACE('',#5172,0.35);
#4465=CYLINDRICAL_SURFACE('',#5175,0.2);
#4466=CYLINDRICAL_SURFACE('',#5178,0.1954);
#4467=CYLINDRICAL_SURFACE('',#5180,0.1954);
#4468=CYLINDRICAL_SURFACE('',#5181,0.1954);
#4469=CYLINDRICAL_SURFACE('',#5182,0.1954);
#4470=CYLINDRICAL_SURFACE('',#5183,0.1954);
#4471=CYLINDRICAL_SURFACE('',#5184,0.1954);
#4472=CYLINDRICAL_SURFACE('',#5185,0.1954);
#4473=CYLINDRICAL_SURFACE('',#5186,0.1954);
#4474=CYLINDRICAL_SURFACE('',#5187,0.1954);
#4475=CYLINDRICAL_SURFACE('',#5188,0.1954);
#4476=CYLINDRICAL_SURFACE('',#5189,0.1954);
#4477=CYLINDRICAL_SURFACE('',#5190,0.1954);
#4478=CYLINDRICAL_SURFACE('',#5191,0.1954);
#4479=CYLINDRICAL_SURFACE('',#5192,0.1954);
#4480=CYLINDRICAL_SURFACE('',#5193,0.1954);
#4481=CYLINDRICAL_SURFACE('',#5194,0.1954);
#4482=CYLINDRICAL_SURFACE('',#5195,0.1954);
#4483=CYLINDRICAL_SURFACE('',#5196,0.1954);
#4484=CYLINDRICAL_SURFACE('',#5197,0.1954);
#4485=CYLINDRICAL_SURFACE('',#5198,0.1954);
#4486=CYLINDRICAL_SURFACE('',#5199,0.1954);
#4487=CYLINDRICAL_SURFACE('',#5200,0.1954);
#4488=CYLINDRICAL_SURFACE('',#5201,0.1954);
#4489=CYLINDRICAL_SURFACE('',#5202,0.1954);
#4490=CYLINDRICAL_SURFACE('',#5203,0.1954);
#4491=CYLINDRICAL_SURFACE('',#5204,0.1954);
#4492=CYLINDRICAL_SURFACE('',#5205,0.1954);
#4493=CYLINDRICAL_SURFACE('',#5206,0.1954);
#4494=CYLINDRICAL_SURFACE('',#5207,0.1954);
#4495=CYLINDRICAL_SURFACE('',#5208,0.1954);
#4496=CYLINDRICAL_SURFACE('',#5209,0.1954);
#4497=CYLINDRICAL_SURFACE('',#5210,0.1954);
#4498=CYLINDRICAL_SURFACE('',#5211,0.1954);
#4499=CYLINDRICAL_SURFACE('',#5212,0.1954);
#4500=CYLINDRICAL_SURFACE('',#5213,0.1954);
#4501=CYLINDRICAL_SURFACE('',#5215,0.15555);
#4502=CYLINDRICAL_SURFACE('',#5217,0.15555);
#4503=CYLINDRICAL_SURFACE('',#5218,0.15555);
#4504=CYLINDRICAL_SURFACE('',#5219,0.15555);
#4505=CYLINDRICAL_SURFACE('',#5220,0.15555);
#4506=CYLINDRICAL_SURFACE('',#5221,0.15555);
#4507=CYLINDRICAL_SURFACE('',#5222,0.15555);
#4508=CYLINDRICAL_SURFACE('',#5223,0.15555);
#4509=CYLINDRICAL_SURFACE('',#5224,0.15555);
#4510=CYLINDRICAL_SURFACE('',#5225,0.15555);
#4511=CYLINDRICAL_SURFACE('',#5226,0.15555);
#4512=CYLINDRICAL_SURFACE('',#5227,0.15555);
#4513=CYLINDRICAL_SURFACE('',#5228,0.15555);
#4514=CYLINDRICAL_SURFACE('',#5229,0.15555);
#4515=CYLINDRICAL_SURFACE('',#5230,0.15555);
#4516=CYLINDRICAL_SURFACE('',#5231,0.15555);
#4517=CYLINDRICAL_SURFACE('',#5232,0.15555);
#4518=CYLINDRICAL_SURFACE('',#5233,0.15555);
#4519=CYLINDRICAL_SURFACE('',#5234,0.15555);
#4520=CYLINDRICAL_SURFACE('',#5235,0.15555);
#4521=CYLINDRICAL_SURFACE('',#5236,0.15555);
#4522=CYLINDRICAL_SURFACE('',#5237,0.15555);
#4523=CYLINDRICAL_SURFACE('',#5238,0.15555);
#4524=CYLINDRICAL_SURFACE('',#5239,0.15555);
#4525=CYLINDRICAL_SURFACE('',#5240,0.15555);
#4526=CYLINDRICAL_SURFACE('',#5241,0.15555);
#4527=CYLINDRICAL_SURFACE('',#5242,0.15555);
#4528=CYLINDRICAL_SURFACE('',#5243,0.15555);
#4529=CYLINDRICAL_SURFACE('',#5244,0.15555);
#4530=CYLINDRICAL_SURFACE('',#5245,0.15555);
#4531=CYLINDRICAL_SURFACE('',#5246,0.15555);
#4532=CYLINDRICAL_SURFACE('',#5247,0.15555);
#4533=CYLINDRICAL_SURFACE('',#5248,0.15555);
#4534=CYLINDRICAL_SURFACE('',#5249,0.15555);
#4535=CYLINDRICAL_SURFACE('',#5250,0.15555);
#4536=CYLINDRICAL_SURFACE('',#5252,0.1954);
#4537=CYLINDRICAL_SURFACE('',#5263,0.4);
#4538=CYLINDRICAL_SURFACE('',#5268,0.1666);
#4539=CYLINDRICAL_SURFACE('',#5270,0.1666);
#4540=CYLINDRICAL_SURFACE('',#5272,0.1666);
#4541=CYLINDRICAL_SURFACE('',#5273,0.1666);
#4542=CYLINDRICAL_SURFACE('',#5274,0.1666);
#4543=CYLINDRICAL_SURFACE('',#5275,0.1666);
#4544=CYLINDRICAL_SURFACE('',#5277,0.205475);
#4545=CYLINDRICAL_SURFACE('',#5279,0.205475);
#4546=CYLINDRICAL_SURFACE('',#5280,0.205475);
#4547=CYLINDRICAL_SURFACE('',#5281,0.205475);
#4548=CYLINDRICAL_SURFACE('',#5282,0.205475);
#4549=CYLINDRICAL_SURFACE('',#5283,0.205475);
#4550=CYLINDRICAL_SURFACE('',#5285,0.205475);
#4551=CYLINDRICAL_SURFACE('',#5287,0.1666);
#4552=CYLINDRICAL_SURFACE('',#5296,0.4);
#4553=ADVANCED_FACE('',(#572),#4432,.F.);
#4554=ADVANCED_FACE('',(#573,#399),#441,.F.);
#4555=ADVANCED_FACE('',(#574),#4433,.F.);
#4556=ADVANCED_FACE('',(#575,#400),#442,.F.);
#4557=ADVANCED_FACE('',(#576),#4434,.F.);
#4558=ADVANCED_FACE('',(#577),#443,.F.);
#4559=ADVANCED_FACE('',(#578),#4435,.F.);
#4560=ADVANCED_FACE('',(#579),#444,.F.);
#4561=ADVANCED_FACE('',(#580),#4436,.F.);
#4562=ADVANCED_FACE('',(#581),#445,.F.);
#4563=ADVANCED_FACE('',(#582),#4437,.F.);
#4564=ADVANCED_FACE('',(#583),#446,.F.);
#4565=ADVANCED_FACE('',(#584),#4438,.F.);
#4566=ADVANCED_FACE('',(#585),#4439,.F.);
#4567=ADVANCED_FACE('',(#586),#447,.F.);
#4568=ADVANCED_FACE('',(#587),#448,.F.);
#4569=ADVANCED_FACE('',(#588),#449,.F.);
#4570=ADVANCED_FACE('',(#589),#450,.F.);
#4571=ADVANCED_FACE('',(#590),#451,.F.);
#4572=ADVANCED_FACE('',(#591),#452,.T.);
#4573=ADVANCED_FACE('',(#592),#453,.T.);
#4574=ADVANCED_FACE('',(#593,#401),#454,.T.);
#4575=ADVANCED_FACE('',(#594),#455,.T.);
#4576=ADVANCED_FACE('',(#595),#456,.F.);
#4577=ADVANCED_FACE('',(#596),#457,.F.);
#4578=ADVANCED_FACE('',(#597),#458,.T.);
#4579=ADVANCED_FACE('',(#598),#459,.T.);
#4580=ADVANCED_FACE('',(#599,#402),#460,.T.);
#4581=ADVANCED_FACE('',(#600),#461,.T.);
#4582=ADVANCED_FACE('',(#601),#462,.F.);
#4583=ADVANCED_FACE('',(#602),#463,.F.);
#4584=ADVANCED_FACE('',(#603),#464,.T.);
#4585=ADVANCED_FACE('',(#604),#465,.F.);
#4586=ADVANCED_FACE('',(#605),#466,.T.);
#4587=ADVANCED_FACE('',(#606,#403,#404,#405,#406,#407,#408),#467,.T.);
#4588=ADVANCED_FACE('',(#607),#468,.T.);
#4589=ADVANCED_FACE('',(#608),#4440,.F.);
#4590=ADVANCED_FACE('',(#609),#469,.F.);
#4591=ADVANCED_FACE('',(#610),#4441,.F.);
#4592=ADVANCED_FACE('',(#611),#470,.F.);
#4593=ADVANCED_FACE('',(#612),#4442,.F.);
#4594=ADVANCED_FACE('',(#613),#471,.F.);
#4595=ADVANCED_FACE('',(#614),#4443,.F.);
#4596=ADVANCED_FACE('',(#615),#472,.F.);
#4597=ADVANCED_FACE('',(#616),#4444,.F.);
#4598=ADVANCED_FACE('',(#617),#4445,.F.);
#4599=ADVANCED_FACE('',(#618),#473,.F.);
#4600=ADVANCED_FACE('',(#619),#474,.F.);
#4601=ADVANCED_FACE('',(#620),#475,.F.);
#4602=ADVANCED_FACE('',(#621),#476,.F.);
#4603=ADVANCED_FACE('',(#622),#477,.F.);
#4604=ADVANCED_FACE('',(#623),#478,.T.);
#4605=ADVANCED_FACE('',(#624),#479,.T.);
#4606=ADVANCED_FACE('',(#625,#409),#480,.T.);
#4607=ADVANCED_FACE('',(#626),#481,.T.);
#4608=ADVANCED_FACE('',(#627),#482,.F.);
#4609=ADVANCED_FACE('',(#628),#483,.F.);
#4610=ADVANCED_FACE('',(#629),#484,.T.);
#4611=ADVANCED_FACE('',(#630),#485,.T.);
#4612=ADVANCED_FACE('',(#631,#410),#486,.T.);
#4613=ADVANCED_FACE('',(#632),#487,.T.);
#4614=ADVANCED_FACE('',(#633),#488,.F.);
#4615=ADVANCED_FACE('',(#634),#489,.F.);
#4616=ADVANCED_FACE('',(#635),#490,.T.);
#4617=ADVANCED_FACE('',(#636),#491,.F.);
#4618=ADVANCED_FACE('',(#637),#492,.T.);
#4619=ADVANCED_FACE('',(#638,#411,#412,#413,#414,#415,#416),#493,.T.);
#4620=ADVANCED_FACE('',(#639),#494,.T.);
#4621=ADVANCED_FACE('',(#640),#495,.F.);
#4622=ADVANCED_FACE('',(#641),#496,.F.);
#4623=ADVANCED_FACE('',(#642),#497,.T.);
#4624=ADVANCED_FACE('',(#643),#498,.T.);
#4625=ADVANCED_FACE('',(#644),#499,.T.);
#4626=ADVANCED_FACE('',(#645),#500,.T.);
#4627=ADVANCED_FACE('',(#646),#501,.T.);
#4628=ADVANCED_FACE('',(#647),#502,.T.);
#4629=ADVANCED_FACE('',(#648),#503,.T.);
#4630=ADVANCED_FACE('',(#649),#504,.F.);
#4631=ADVANCED_FACE('',(#650),#505,.T.);
#4632=ADVANCED_FACE('',(#651),#506,.T.);
#4633=ADVANCED_FACE('',(#652),#507,.T.);
#4634=ADVANCED_FACE('',(#653),#508,.T.);
#4635=ADVANCED_FACE('',(#654),#509,.T.);
#4636=ADVANCED_FACE('',(#655),#510,.F.);
#4637=ADVANCED_FACE('',(#656),#511,.F.);
#4638=ADVANCED_FACE('',(#657),#512,.F.);
#4639=ADVANCED_FACE('',(#658),#513,.T.);
#4640=ADVANCED_FACE('',(#659),#514,.T.);
#4641=ADVANCED_FACE('',(#660),#515,.T.);
#4642=ADVANCED_FACE('',(#661),#516,.T.);
#4643=ADVANCED_FACE('',(#662),#517,.T.);
#4644=ADVANCED_FACE('',(#663),#518,.F.);
#4645=ADVANCED_FACE('',(#664),#519,.F.);
#4646=ADVANCED_FACE('',(#665),#4446,.F.);
#4647=ADVANCED_FACE('',(#666),#520,.F.);
#4648=ADVANCED_FACE('',(#667),#4447,.F.);
#4649=ADVANCED_FACE('',(#668),#4448,.F.);
#4650=ADVANCED_FACE('',(#669),#4449,.F.);
#4651=ADVANCED_FACE('',(#670,#417,#418,#419),#521,.T.);
#4652=ADVANCED_FACE('',(#671),#522,.T.);
#4653=ADVANCED_FACE('',(#672,#420,#421,#422),#523,.T.);
#4654=ADVANCED_FACE('',(#673),#524,.T.);
#4655=ADVANCED_FACE('',(#674),#525,.T.);
#4656=ADVANCED_FACE('',(#675),#526,.F.);
#4657=ADVANCED_FACE('',(#676),#4450,.F.);
#4658=ADVANCED_FACE('',(#677),#4451,.F.);
#4659=ADVANCED_FACE('',(#678),#527,.F.);
#4660=ADVANCED_FACE('',(#679),#4452,.F.);
#4661=ADVANCED_FACE('',(#680),#528,.T.);
#4662=ADVANCED_FACE('',(#681,#423,#424),#529,.T.);
#4663=ADVANCED_FACE('',(#682),#530,.T.);
#4664=ADVANCED_FACE('',(#683),#531,.T.);
#4665=ADVANCED_FACE('',(#684),#532,.F.);
#4666=ADVANCED_FACE('',(#685),#4453,.T.);
#4667=ADVANCED_FACE('',(#686),#4454,.F.);
#4668=ADVANCED_FACE('',(#687,#425),#533,.T.);
#4669=ADVANCED_FACE('',(#688,#426,#427),#534,.T.);
#4670=ADVANCED_FACE('',(#689),#4455,.F.);
#4671=ADVANCED_FACE('',(#690),#4456,.T.);
#4672=ADVANCED_FACE('',(#691),#535,.T.);
#4673=ADVANCED_FACE('',(#692),#536,.T.);
#4674=ADVANCED_FACE('',(#693,#428),#537,.F.);
#4675=ADVANCED_FACE('',(#694),#4457,.F.);
#4676=ADVANCED_FACE('',(#695),#4458,.F.);
#4677=ADVANCED_FACE('',(#696),#538,.T.);
#4678=ADVANCED_FACE('',(#697),#4459,.F.);
#4679=ADVANCED_FACE('',(#698,#429,#430),#539,.T.);
#4680=ADVANCED_FACE('',(#699),#540,.T.);
#4681=ADVANCED_FACE('',(#700),#4460,.F.);
#4682=ADVANCED_FACE('',(#701),#541,.F.);
#4683=ADVANCED_FACE('',(#702),#542,.F.);
#4684=ADVANCED_FACE('',(#703,#431),#543,.T.);
#4685=ADVANCED_FACE('',(#704),#4461,.F.);
#4686=ADVANCED_FACE('',(#705),#4462,.T.);
#4687=ADVANCED_FACE('',(#706,#432),#544,.F.);
#4688=ADVANCED_FACE('',(#707,#433,#434),#545,.T.);
#4689=ADVANCED_FACE('',(#708),#546,.T.);
#4690=ADVANCED_FACE('',(#709),#547,.T.);
#4691=ADVANCED_FACE('',(#710,#435),#548,.F.);
#4692=ADVANCED_FACE('',(#711),#4463,.T.);
#4693=ADVANCED_FACE('',(#712,#436),#549,.T.);
#4694=ADVANCED_FACE('',(#713),#4464,.T.);
#4695=ADVANCED_FACE('',(#714),#550,.F.);
#4696=ADVANCED_FACE('',(#715),#4465,.T.);
#4697=ADVANCED_FACE('',(#716),#551,.T.);
#4698=ADVANCED_FACE('',(#717),#4466,.T.);
#4699=ADVANCED_FACE('',(#718),#4467,.T.);
#4700=ADVANCED_FACE('',(#719),#4468,.T.);
#4701=ADVANCED_FACE('',(#720),#4469,.T.);
#4702=ADVANCED_FACE('',(#721),#4470,.T.);
#4703=ADVANCED_FACE('',(#722),#4471,.T.);
#4704=ADVANCED_FACE('',(#723),#4472,.T.);
#4705=ADVANCED_FACE('',(#724),#4473,.T.);
#4706=ADVANCED_FACE('',(#725),#4474,.T.);
#4707=ADVANCED_FACE('',(#726),#4475,.T.);
#4708=ADVANCED_FACE('',(#727),#4476,.T.);
#4709=ADVANCED_FACE('',(#728),#4477,.T.);
#4710=ADVANCED_FACE('',(#729),#4478,.T.);
#4711=ADVANCED_FACE('',(#730),#4479,.T.);
#4712=ADVANCED_FACE('',(#731),#4480,.T.);
#4713=ADVANCED_FACE('',(#732),#4481,.T.);
#4714=ADVANCED_FACE('',(#733),#4482,.T.);
#4715=ADVANCED_FACE('',(#734),#4483,.T.);
#4716=ADVANCED_FACE('',(#735),#4484,.T.);
#4717=ADVANCED_FACE('',(#736),#4485,.T.);
#4718=ADVANCED_FACE('',(#737),#4486,.T.);
#4719=ADVANCED_FACE('',(#738),#4487,.T.);
#4720=ADVANCED_FACE('',(#739),#4488,.T.);
#4721=ADVANCED_FACE('',(#740),#4489,.T.);
#4722=ADVANCED_FACE('',(#741),#4490,.T.);
#4723=ADVANCED_FACE('',(#742),#4491,.T.);
#4724=ADVANCED_FACE('',(#743),#4492,.T.);
#4725=ADVANCED_FACE('',(#744),#4493,.T.);
#4726=ADVANCED_FACE('',(#745),#4494,.T.);
#4727=ADVANCED_FACE('',(#746),#4495,.T.);
#4728=ADVANCED_FACE('',(#747),#4496,.T.);
#4729=ADVANCED_FACE('',(#748),#4497,.T.);
#4730=ADVANCED_FACE('',(#749),#4498,.T.);
#4731=ADVANCED_FACE('',(#750),#4499,.T.);
#4732=ADVANCED_FACE('',(#751),#4500,.T.);
#4733=ADVANCED_FACE('',(#752),#4501,.T.);
#4734=ADVANCED_FACE('',(#753),#4502,.T.);
#4735=ADVANCED_FACE('',(#754),#4503,.T.);
#4736=ADVANCED_FACE('',(#755),#4504,.T.);
#4737=ADVANCED_FACE('',(#756),#4505,.T.);
#4738=ADVANCED_FACE('',(#757),#4506,.T.);
#4739=ADVANCED_FACE('',(#758),#4507,.T.);
#4740=ADVANCED_FACE('',(#759),#4508,.T.);
#4741=ADVANCED_FACE('',(#760),#4509,.T.);
#4742=ADVANCED_FACE('',(#761),#4510,.T.);
#4743=ADVANCED_FACE('',(#762),#4511,.T.);
#4744=ADVANCED_FACE('',(#763),#4512,.T.);
#4745=ADVANCED_FACE('',(#764),#4513,.T.);
#4746=ADVANCED_FACE('',(#765),#4514,.T.);
#4747=ADVANCED_FACE('',(#766),#4515,.T.);
#4748=ADVANCED_FACE('',(#767),#4516,.T.);
#4749=ADVANCED_FACE('',(#768),#4517,.T.);
#4750=ADVANCED_FACE('',(#769),#4518,.T.);
#4751=ADVANCED_FACE('',(#770),#4519,.T.);
#4752=ADVANCED_FACE('',(#771),#4520,.T.);
#4753=ADVANCED_FACE('',(#772),#4521,.T.);
#4754=ADVANCED_FACE('',(#773),#4522,.T.);
#4755=ADVANCED_FACE('',(#774),#4523,.T.);
#4756=ADVANCED_FACE('',(#775),#4524,.T.);
#4757=ADVANCED_FACE('',(#776),#4525,.T.);
#4758=ADVANCED_FACE('',(#777),#4526,.T.);
#4759=ADVANCED_FACE('',(#778),#4527,.T.);
#4760=ADVANCED_FACE('',(#779),#4528,.T.);
#4761=ADVANCED_FACE('',(#780),#4529,.T.);
#4762=ADVANCED_FACE('',(#781),#4530,.T.);
#4763=ADVANCED_FACE('',(#782),#4531,.T.);
#4764=ADVANCED_FACE('',(#783),#4532,.T.);
#4765=ADVANCED_FACE('',(#784),#4533,.T.);
#4766=ADVANCED_FACE('',(#785),#4534,.T.);
#4767=ADVANCED_FACE('',(#786),#171,.F.);
#4768=ADVANCED_FACE('',(#787),#4535,.T.);
#4769=ADVANCED_FACE('',(#788),#172,.F.);
#4770=ADVANCED_FACE('',(#789),#4536,.T.);
#4771=ADVANCED_FACE('',(#790),#552,.F.);
#4772=ADVANCED_FACE('',(#791),#553,.F.);
#4773=ADVANCED_FACE('',(#792),#554,.F.);
#4774=ADVANCED_FACE('',(#793),#555,.F.);
#4775=ADVANCED_FACE('',(#794),#556,.F.);
#4776=ADVANCED_FACE('',(#795),#557,.F.);
#4777=ADVANCED_FACE('',(#796),#558,.F.);
#4778=ADVANCED_FACE('',(#797,#437),#559,.T.);
#4779=ADVANCED_FACE('',(#798),#4537,.T.);
#4780=ADVANCED_FACE('',(#799,#438),#560,.F.);
#4781=ADVANCED_FACE('',(#800),#561,.T.);
#4782=ADVANCED_FACE('',(#801),#4538,.F.);
#4783=ADVANCED_FACE('',(#802),#4539,.F.);
#4784=ADVANCED_FACE('',(#803),#4540,.F.);
#4785=ADVANCED_FACE('',(#804),#4541,.F.);
#4786=ADVANCED_FACE('',(#805),#4542,.F.);
#4787=ADVANCED_FACE('',(#806),#4543,.F.);
#4788=ADVANCED_FACE('',(#807),#4544,.F.);
#4789=ADVANCED_FACE('',(#808),#4545,.F.);
#4790=ADVANCED_FACE('',(#809),#4546,.F.);
#4791=ADVANCED_FACE('',(#810),#4547,.F.);
#4792=ADVANCED_FACE('',(#811),#4548,.F.);
#4793=ADVANCED_FACE('',(#812),#4549,.F.);
#4794=ADVANCED_FACE('',(#813),#4550,.F.);
#4795=ADVANCED_FACE('',(#814),#173,.F.);
#4796=ADVANCED_FACE('',(#815),#174,.F.);
#4797=ADVANCED_FACE('',(#816,#439),#562,.T.);
#4798=ADVANCED_FACE('',(#817),#4551,.F.);
#4799=ADVANCED_FACE('',(#818),#563,.T.);
#4800=ADVANCED_FACE('',(#819),#564,.T.);
#4801=ADVANCED_FACE('',(#820),#565,.T.);
#4802=ADVANCED_FACE('',(#821),#566,.T.);
#4803=ADVANCED_FACE('',(#822),#567,.T.);
#4804=ADVANCED_FACE('',(#823),#568,.T.);
#4805=ADVANCED_FACE('',(#824,#440),#569,.F.);
#4806=ADVANCED_FACE('',(#825),#4552,.T.);
#4807=ADVANCED_FACE('',(#826),#570,.T.);
#4808=ADVANCED_FACE('',(#827),#571,.F.);
#4809=CLOSED_SHELL('',(#4553,#4554,#4555,#4556,#4557,#4558,#4559,#4560,
#4561,#4562,#4563,#4564,#4565,#4566,#4567,#4568,#4569,#4570,#4571,#4572,
#4573,#4574,#4575,#4576,#4577,#4578,#4579,#4580,#4581,#4582,#4583,#4584,
#4585,#4586,#4587,#4588));
#4810=CLOSED_SHELL('',(#4589,#4590,#4591,#4592,#4593,#4594,#4595,#4596,
#4597,#4598,#4599,#4600,#4601,#4602,#4603,#4604,#4605,#4606,#4607,#4608,
#4609,#4610,#4611,#4612,#4613,#4614,#4615,#4616,#4617,#4618,#4619,#4620));
#4811=CLOSED_SHELL('',(#4621,#4622,#4623,#4624,#4625,#4626,#4627,#4628,
#4629,#4630));
#4812=CLOSED_SHELL('',(#4631,#4632,#4633,#4634,#4635,#4636));
#4813=CLOSED_SHELL('',(#4637,#4638,#4639,#4640,#4641,#4642,#4643,#4644));
#4814=CLOSED_SHELL('',(#4645,#4646,#4647,#4648,#4649,#4650,#4651,#4652,
#4653,#4654,#4655,#4656));
#4815=CLOSED_SHELL('',(#4657,#4658,#4659,#4660,#4661,#4662,#4663,#4664,
#4665,#4666,#4667,#4668,#4669,#4670,#4671,#4672,#4673,#4674));
#4816=CLOSED_SHELL('',(#4675,#4676,#4677,#4678,#4679,#4680,#4681,#4682,
#4683,#4684,#4685,#4686,#4687,#4688,#4689,#4690));
#4817=CLOSED_SHELL('',(#4691,#4692,#4693,#4694,#4695,#4696,#4697));
#4818=CLOSED_SHELL('',(#4698,#4699,#4700,#4701,#4702,#4703,#4704,#4705,
#4706,#4707,#4708,#4709,#4710,#4711,#4712,#4713,#4714,#4715,#4716,#4717,
#4718,#4719,#4720,#4721,#4722,#4723,#4724,#4725,#4726,#4727,#4728,#4729,
#4730,#4731,#4732,#4733,#4734,#4735,#4736,#4737,#4738,#4739,#4740,#4741,
#4742,#4743,#4744,#4745,#4746,#4747,#4748,#4749,#4750,#4751,#4752,#4753,
#4754,#4755,#4756,#4757,#4758,#4759,#4760,#4761,#4762,#4763,#4764,#4765,
#4766,#4767,#4768,#4769,#4770,#4771,#4772,#4773,#4774,#4775,#4776,#4777,
#4778,#4779,#4780,#4781));
#4819=CLOSED_SHELL('',(#4782,#4783,#4784,#4785,#4786,#4787,#4788,#4789,
#4790,#4791,#4792,#4793,#4794,#4795,#4796,#4797,#4798,#4799,#4800,#4801,
#4802,#4803,#4804,#4805));
#4820=CLOSED_SHELL('',(#4806,#4807,#4808));
#4821=DERIVED_UNIT_ELEMENT(#4845,1.);
#4822=DERIVED_UNIT_ELEMENT(#12965,-3.);
#4823=DERIVED_UNIT_ELEMENT(#4845,1.);
#4824=DERIVED_UNIT_ELEMENT(#12965,-3.);
#4825=DERIVED_UNIT_ELEMENT(#4845,1.);
#4826=DERIVED_UNIT_ELEMENT(#12965,-3.);
#4827=DERIVED_UNIT_ELEMENT(#4845,1.);
#4828=DERIVED_UNIT_ELEMENT(#12965,-3.);
#4829=DERIVED_UNIT_ELEMENT(#4845,1.);
#4830=DERIVED_UNIT_ELEMENT(#12965,-3.);
#4831=DERIVED_UNIT_ELEMENT(#4845,1.);
#4832=DERIVED_UNIT_ELEMENT(#12965,-3.);
#4833=DERIVED_UNIT_ELEMENT(#4845,1.);
#4834=DERIVED_UNIT_ELEMENT(#12965,-3.);
#4835=DERIVED_UNIT_ELEMENT(#4845,1.);
#4836=DERIVED_UNIT_ELEMENT(#12965,-3.);
#4837=DERIVED_UNIT_ELEMENT(#4845,1.);
#4838=DERIVED_UNIT_ELEMENT(#12965,-3.);
#4839=DERIVED_UNIT_ELEMENT(#4845,1.);
#4840=DERIVED_UNIT_ELEMENT(#12965,-3.);
#4841=DERIVED_UNIT_ELEMENT(#4845,1.);
#4842=DERIVED_UNIT_ELEMENT(#12965,-3.);
#4843=DERIVED_UNIT_ELEMENT(#4845,1.);
#4844=DERIVED_UNIT_ELEMENT(#12965,-3.);
#4845=(
MASS_UNIT()
NAMED_UNIT(*)
SI_UNIT(.KILO.,.GRAM.)
);
#4846=DERIVED_UNIT((#4821,#4822));
#4847=DERIVED_UNIT((#4823,#4824));
#4848=DERIVED_UNIT((#4825,#4826));
#4849=DERIVED_UNIT((#4827,#4828));
#4850=DERIVED_UNIT((#4829,#4830));
#4851=DERIVED_UNIT((#4831,#4832));
#4852=DERIVED_UNIT((#4833,#4834));
#4853=DERIVED_UNIT((#4835,#4836));
#4854=DERIVED_UNIT((#4837,#4838));
#4855=DERIVED_UNIT((#4839,#4840));
#4856=DERIVED_UNIT((#4841,#4842));
#4857=DERIVED_UNIT((#4843,#4844));
#4858=MEASURE_REPRESENTATION_ITEM('density measure',
POSITIVE_RATIO_MEASURE(7850.),#4846);
#4859=MEASURE_REPRESENTATION_ITEM('density measure',
POSITIVE_RATIO_MEASURE(7850.),#4847);
#4860=MEASURE_REPRESENTATION_ITEM('density measure',
POSITIVE_RATIO_MEASURE(7850.),#4848);
#4861=MEASURE_REPRESENTATION_ITEM('density measure',
POSITIVE_RATIO_MEASURE(7850.),#4849);
#4862=MEASURE_REPRESENTATION_ITEM('density measure',
POSITIVE_RATIO_MEASURE(7850.),#4850);
#4863=MEASURE_REPRESENTATION_ITEM('density measure',
POSITIVE_RATIO_MEASURE(7850.),#4851);
#4864=MEASURE_REPRESENTATION_ITEM('density measure',
POSITIVE_RATIO_MEASURE(7850.),#4852);
#4865=MEASURE_REPRESENTATION_ITEM('density measure',
POSITIVE_RATIO_MEASURE(7850.),#4853);
#4866=MEASURE_REPRESENTATION_ITEM('density measure',
POSITIVE_RATIO_MEASURE(7850.),#4854);
#4867=MEASURE_REPRESENTATION_ITEM('density measure',
POSITIVE_RATIO_MEASURE(7850.),#4855);
#4868=MEASURE_REPRESENTATION_ITEM('density measure',
POSITIVE_RATIO_MEASURE(7850.),#4856);
#4869=MEASURE_REPRESENTATION_ITEM('density measure',
POSITIVE_RATIO_MEASURE(7850.),#4857);
#4870=PROPERTY_DEFINITION_REPRESENTATION(#4930,#4894);
#4871=PROPERTY_DEFINITION_REPRESENTATION(#4931,#4895);
#4872=PROPERTY_DEFINITION_REPRESENTATION(#4932,#4896);
#4873=PROPERTY_DEFINITION_REPRESENTATION(#4933,#4897);
#4874=PROPERTY_DEFINITION_REPRESENTATION(#4934,#4898);
#4875=PROPERTY_DEFINITION_REPRESENTATION(#4935,#4899);
#4876=PROPERTY_DEFINITION_REPRESENTATION(#4936,#4900);
#4877=PROPERTY_DEFINITION_REPRESENTATION(#4937,#4901);
#4878=PROPERTY_DEFINITION_REPRESENTATION(#4938,#4902);
#4879=PROPERTY_DEFINITION_REPRESENTATION(#4939,#4903);
#4880=PROPERTY_DEFINITION_REPRESENTATION(#4940,#4904);
#4881=PROPERTY_DEFINITION_REPRESENTATION(#4941,#4905);
#4882=PROPERTY_DEFINITION_REPRESENTATION(#4942,#4906);
#4883=PROPERTY_DEFINITION_REPRESENTATION(#4943,#4907);
#4884=PROPERTY_DEFINITION_REPRESENTATION(#4944,#4908);
#4885=PROPERTY_DEFINITION_REPRESENTATION(#4945,#4909);
#4886=PROPERTY_DEFINITION_REPRESENTATION(#4946,#4910);
#4887=PROPERTY_DEFINITION_REPRESENTATION(#4947,#4911);
#4888=PROPERTY_DEFINITION_REPRESENTATION(#4948,#4912);
#4889=PROPERTY_DEFINITION_REPRESENTATION(#4949,#4913);
#4890=PROPERTY_DEFINITION_REPRESENTATION(#4950,#4914);
#4891=PROPERTY_DEFINITION_REPRESENTATION(#4951,#4915);
#4892=PROPERTY_DEFINITION_REPRESENTATION(#4952,#4916);
#4893=PROPERTY_DEFINITION_REPRESENTATION(#4953,#4917);
#4894=REPRESENTATION('material name',(#4918),#12951);
#4895=REPRESENTATION('density',(#4858),#12951);
#4896=REPRESENTATION('material name',(#4919),#12952);
#4897=REPRESENTATION('density',(#4859),#12952);
#4898=REPRESENTATION('material name',(#4920),#12953);
#4899=REPRESENTATION('density',(#4860),#12953);
#4900=REPRESENTATION('material name',(#4921),#12954);
#4901=REPRESENTATION('density',(#4861),#12954);
#4902=REPRESENTATION('material name',(#4922),#12955);
#4903=REPRESENTATION('density',(#4862),#12955);
#4904=REPRESENTATION('material name',(#4923),#12956);
#4905=REPRESENTATION('density',(#4863),#12956);
#4906=REPRESENTATION('material name',(#4924),#12957);
#4907=REPRESENTATION('density',(#4864),#12957);
#4908=REPRESENTATION('material name',(#4925),#12958);
#4909=REPRESENTATION('density',(#4865),#12958);
#4910=REPRESENTATION('material name',(#4926),#12959);
#4911=REPRESENTATION('density',(#4866),#12959);
#4912=REPRESENTATION('material name',(#4927),#12960);
#4913=REPRESENTATION('density',(#4867),#12960);
#4914=REPRESENTATION('material name',(#4928),#12961);
#4915=REPRESENTATION('density',(#4868),#12961);
#4916=REPRESENTATION('material name',(#4929),#12962);
#4917=REPRESENTATION('density',(#4869),#12962);
#4918=DESCRIPTIVE_REPRESENTATION_ITEM('Steel','Steel');
#4919=DESCRIPTIVE_REPRESENTATION_ITEM('Steel','Steel');
#4920=DESCRIPTIVE_REPRESENTATION_ITEM('Steel','Steel');
#4921=DESCRIPTIVE_REPRESENTATION_ITEM('Steel','Steel');
#4922=DESCRIPTIVE_REPRESENTATION_ITEM('Steel','Steel');
#4923=DESCRIPTIVE_REPRESENTATION_ITEM('Steel','Steel');
#4924=DESCRIPTIVE_REPRESENTATION_ITEM('Steel','Steel');
#4925=DESCRIPTIVE_REPRESENTATION_ITEM('Steel','Steel');
#4926=DESCRIPTIVE_REPRESENTATION_ITEM('Steel','Steel');
#4927=DESCRIPTIVE_REPRESENTATION_ITEM('Steel','Steel');
#4928=DESCRIPTIVE_REPRESENTATION_ITEM('Steel','Steel');
#4929=DESCRIPTIVE_REPRESENTATION_ITEM('Steel','Steel');
#4930=PROPERTY_DEFINITION('material property','material name',#13049);
#4931=PROPERTY_DEFINITION('material property','density of part',#13049);
#4932=PROPERTY_DEFINITION('material property','material name',#13050);
#4933=PROPERTY_DEFINITION('material property','density of part',#13050);
#4934=PROPERTY_DEFINITION('material property','material name',#13051);
#4935=PROPERTY_DEFINITION('material property','density of part',#13051);
#4936=PROPERTY_DEFINITION('material property','material name',#13052);
#4937=PROPERTY_DEFINITION('material property','density of part',#13052);
#4938=PROPERTY_DEFINITION('material property','material name',#13053);
#4939=PROPERTY_DEFINITION('material property','density of part',#13053);
#4940=PROPERTY_DEFINITION('material property','material name',#13054);
#4941=PROPERTY_DEFINITION('material property','density of part',#13054);
#4942=PROPERTY_DEFINITION('material property','material name',#13055);
#4943=PROPERTY_DEFINITION('material property','density of part',#13055);
#4944=PROPERTY_DEFINITION('material property','material name',#13056);
#4945=PROPERTY_DEFINITION('material property','density of part',#13056);
#4946=PROPERTY_DEFINITION('material property','material name',#13057);
#4947=PROPERTY_DEFINITION('material property','density of part',#13057);
#4948=PROPERTY_DEFINITION('material property','material name',#13058);
#4949=PROPERTY_DEFINITION('material property','density of part',#13058);
#4950=PROPERTY_DEFINITION('material property','material name',#13059);
#4951=PROPERTY_DEFINITION('material property','density of part',#13059);
#4952=PROPERTY_DEFINITION('material property','material name',#13060);
#4953=PROPERTY_DEFINITION('material property','density of part',#13060);
#4954=AXIS2_PLACEMENT_3D('',#6517,#5341,#5342);
#4955=AXIS2_PLACEMENT_3D('',#6518,#5343,#5344);
#4956=AXIS2_PLACEMENT_3D('',#6519,#5345,#5346);
#4957=AXIS2_PLACEMENT_3D('',#6521,#5347,#5348);
#4958=AXIS2_PLACEMENT_3D('',#6524,#5350,#5351);
#4959=AXIS2_PLACEMENT_3D('',#6525,#5352,#5353);
#4960=AXIS2_PLACEMENT_3D('',#6527,#5354,#5355);
#4961=AXIS2_PLACEMENT_3D('',#6528,#5356,#5357);
#4962=AXIS2_PLACEMENT_3D('',#6530,#5358,#5359);
#4963=AXIS2_PLACEMENT_3D('',#6533,#5361,#5362);
#4964=AXIS2_PLACEMENT_3D('',#6534,#5363,#5364);
#4965=AXIS2_PLACEMENT_3D('',#6536,#5365,#5366);
#4966=AXIS2_PLACEMENT_3D('',#6537,#5367,#5368);
#4967=AXIS2_PLACEMENT_3D('',#6539,#5369,#5370);
#4968=AXIS2_PLACEMENT_3D('',#6542,#5372,#5373);
#4969=AXIS2_PLACEMENT_3D('',#6543,#5374,#5375);
#4970=AXIS2_PLACEMENT_3D('',#6544,#5376,#5377);
#4971=AXIS2_PLACEMENT_3D('',#6546,#5378,#5379);
#4972=AXIS2_PLACEMENT_3D('',#6549,#5381,#5382);
#4973=AXIS2_PLACEMENT_3D('',#6550,#5383,#5384);
#4974=AXIS2_PLACEMENT_3D('',#6551,#5385,#5386);
#4975=AXIS2_PLACEMENT_3D('',#6553,#5387,#5388);
#4976=AXIS2_PLACEMENT_3D('',#6556,#5390,#5391);
#4977=AXIS2_PLACEMENT_3D('',#6557,#5392,#5393);
#4978=AXIS2_PLACEMENT_3D('',#6558,#5394,#5395);
#4979=AXIS2_PLACEMENT_3D('',#6560,#5396,#5397);
#4980=AXIS2_PLACEMENT_3D('',#6563,#5399,#5400);
#4981=AXIS2_PLACEMENT_3D('',#6564,#5401,#5402);
#4982=AXIS2_PLACEMENT_3D('',#6565,#5403,#5404);
#4983=AXIS2_PLACEMENT_3D('',#6567,#5405,#5406);
#4984=AXIS2_PLACEMENT_3D('',#6569,#5408,#5409);
#4985=AXIS2_PLACEMENT_3D('',#6571,#5410,#5411);
#4986=AXIS2_PLACEMENT_3D('',#6573,#5413,#5414);
#4987=AXIS2_PLACEMENT_3D('',#6582,#5419,#5420);
#4988=AXIS2_PLACEMENT_3D('',#6591,#5425,#5426);
#4989=AXIS2_PLACEMENT_3D('',#6600,#5431,#5432);
#4990=AXIS2_PLACEMENT_3D('',#6609,#5437,#5438);
#4991=AXIS2_PLACEMENT_3D('',#6638,#5455,#5456);
#4992=AXIS2_PLACEMENT_3D('',#6642,#5459,#5460);
#4993=AXIS2_PLACEMENT_3D('',#6646,#5463,#5464);
#4994=AXIS2_PLACEMENT_3D('',#6650,#5467,#5468);
#4995=AXIS2_PLACEMENT_3D('',#6654,#5471,#5472);
#4996=AXIS2_PLACEMENT_3D('',#6656,#5474,#5475);
#4997=AXIS2_PLACEMENT_3D('',#6658,#5477,#5478);
#4998=AXIS2_PLACEMENT_3D('',#6662,#5481,#5482);
#4999=AXIS2_PLACEMENT_3D('',#6666,#5485,#5486);
#5000=AXIS2_PLACEMENT_3D('',#6670,#5489,#5490);
#5001=AXIS2_PLACEMENT_3D('',#6674,#5493,#5494);
#5002=AXIS2_PLACEMENT_3D('',#6676,#5496,#5497);
#5003=AXIS2_PLACEMENT_3D('',#6678,#5499,#5500);
#5004=AXIS2_PLACEMENT_3D('',#6684,#5504,#5505);
#5005=AXIS2_PLACEMENT_3D('',#6688,#5508,#5509);
#5006=AXIS2_PLACEMENT_3D('',#6692,#5512,#5513);
#5007=AXIS2_PLACEMENT_3D('',#6694,#5515,#5516);
#5008=AXIS2_PLACEMENT_3D('',#6695,#5517,#5518);
#5009=AXIS2_PLACEMENT_3D('',#6696,#5519,#5520);
#5010=AXIS2_PLACEMENT_3D('',#6698,#5521,#5522);
#5011=AXIS2_PLACEMENT_3D('',#6701,#5524,#5525);
#5012=AXIS2_PLACEMENT_3D('',#6702,#5526,#5527);
#5013=AXIS2_PLACEMENT_3D('',#6703,#5528,#5529);
#5014=AXIS2_PLACEMENT_3D('',#6705,#5530,#5531);
#5015=AXIS2_PLACEMENT_3D('',#6708,#5533,#5534);
#5016=AXIS2_PLACEMENT_3D('',#6709,#5535,#5536);
#5017=AXIS2_PLACEMENT_3D('',#6710,#5537,#5538);
#5018=AXIS2_PLACEMENT_3D('',#6712,#5539,#5540);
#5019=AXIS2_PLACEMENT_3D('',#6715,#5542,#5543);
#5020=AXIS2_PLACEMENT_3D('',#6716,#5544,#5545);
#5021=AXIS2_PLACEMENT_3D('',#6717,#5546,#5547);
#5022=AXIS2_PLACEMENT_3D('',#6719,#5548,#5549);
#5023=AXIS2_PLACEMENT_3D('',#6722,#5551,#5552);
#5024=AXIS2_PLACEMENT_3D('',#6723,#5553,#5554);
#5025=AXIS2_PLACEMENT_3D('',#6724,#5555,#5556);
#5026=AXIS2_PLACEMENT_3D('',#6726,#5557,#5558);
#5027=AXIS2_PLACEMENT_3D('',#6729,#5560,#5561);
#5028=AXIS2_PLACEMENT_3D('',#6730,#5562,#5563);
#5029=AXIS2_PLACEMENT_3D('',#6732,#5564,#5565);
#5030=AXIS2_PLACEMENT_3D('',#6735,#5567,#5568);
#5031=AXIS2_PLACEMENT_3D('',#6736,#5569,#5570);
#5032=AXIS2_PLACEMENT_3D('',#6745,#5575,#5576);
#5033=AXIS2_PLACEMENT_3D('',#6754,#5581,#5582);
#5034=AXIS2_PLACEMENT_3D('',#6763,#5587,#5588);
#5035=AXIS2_PLACEMENT_3D('',#6772,#5593,#5594);
#5036=AXIS2_PLACEMENT_3D('',#6801,#5611,#5612);
#5037=AXIS2_PLACEMENT_3D('',#6805,#5615,#5616);
#5038=AXIS2_PLACEMENT_3D('',#6809,#5619,#5620);
#5039=AXIS2_PLACEMENT_3D('',#6813,#5623,#5624);
#5040=AXIS2_PLACEMENT_3D('',#6817,#5627,#5628);
#5041=AXIS2_PLACEMENT_3D('',#6819,#5630,#5631);
#5042=AXIS2_PLACEMENT_3D('',#6821,#5633,#5634);
#5043=AXIS2_PLACEMENT_3D('',#6825,#5637,#5638);
#5044=AXIS2_PLACEMENT_3D('',#6829,#5641,#5642);
#5045=AXIS2_PLACEMENT_3D('',#6833,#5645,#5646);
#5046=AXIS2_PLACEMENT_3D('',#6837,#5649,#5650);
#5047=AXIS2_PLACEMENT_3D('',#6839,#5652,#5653);
#5048=AXIS2_PLACEMENT_3D('',#6841,#5655,#5656);
#5049=AXIS2_PLACEMENT_3D('',#6847,#5660,#5661);
#5050=AXIS2_PLACEMENT_3D('',#6851,#5664,#5665);
#5051=AXIS2_PLACEMENT_3D('',#6855,#5668,#5669);
#5052=AXIS2_PLACEMENT_3D('',#6857,#5671,#5672);
#5053=AXIS2_PLACEMENT_3D('',#6858,#5673,#5674);
#5054=AXIS2_PLACEMENT_3D('',#6859,#5675,#5676);
#5055=AXIS2_PLACEMENT_3D('',#6868,#5681,#5682);
#5056=AXIS2_PLACEMENT_3D('',#6877,#5687,#5688);
#5057=AXIS2_PLACEMENT_3D('',#6880,#5691,#5692);
#5058=AXIS2_PLACEMENT_3D('',#6890,#5698,#5699);
#5059=AXIS2_PLACEMENT_3D('',#6894,#5702,#5703);
#5060=AXIS2_PLACEMENT_3D('',#6900,#5707,#5708);
#5061=AXIS2_PLACEMENT_3D('',#6904,#5711,#5712);
#5062=AXIS2_PLACEMENT_3D('',#6907,#5715,#5716);
#5063=AXIS2_PLACEMENT_3D('',#6908,#5717,#5718);
#5064=AXIS2_PLACEMENT_3D('',#6909,#5719,#5720);
#5065=AXIS2_PLACEMENT_3D('',#6910,#5721,#5722);
#5066=AXIS2_PLACEMENT_3D('',#6919,#5727,#5728);
#5067=AXIS2_PLACEMENT_3D('',#6925,#5732,#5733);
#5068=AXIS2_PLACEMENT_3D('',#6931,#5737,#5738);
#5069=AXIS2_PLACEMENT_3D('',#6934,#5741,#5742);
#5070=AXIS2_PLACEMENT_3D('',#6935,#5743,#5744);
#5071=AXIS2_PLACEMENT_3D('',#6936,#5745,#5746);
#5072=AXIS2_PLACEMENT_3D('',#6937,#5747,#5748);
#5073=AXIS2_PLACEMENT_3D('',#6946,#5753,#5754);
#5074=AXIS2_PLACEMENT_3D('',#6952,#5758,#5759);
#5075=AXIS2_PLACEMENT_3D('',#6958,#5763,#5764);
#5076=AXIS2_PLACEMENT_3D('',#6964,#5768,#5769);
#5077=AXIS2_PLACEMENT_3D('',#6970,#5773,#5774);
#5078=AXIS2_PLACEMENT_3D('',#6973,#5777,#5778);
#5079=AXIS2_PLACEMENT_3D('',#6974,#5779,#5780);
#5080=AXIS2_PLACEMENT_3D('',#6975,#5781,#5782);
#5081=AXIS2_PLACEMENT_3D('',#6976,#5783,#5784);
#5082=AXIS2_PLACEMENT_3D('',#6985,#5789,#5790);
#5083=AXIS2_PLACEMENT_3D('',#6987,#5791,#5792);
#5084=AXIS2_PLACEMENT_3D('',#6990,#5794,#5795);
#5085=AXIS2_PLACEMENT_3D('',#6991,#5796,#5797);
#5086=AXIS2_PLACEMENT_3D('',#6997,#5801,#5802);
#5087=AXIS2_PLACEMENT_3D('',#6998,#5803,#5804);
#5088=AXIS2_PLACEMENT_3D('',#6999,#5805,#5806);
#5089=AXIS2_PLACEMENT_3D('',#7000,#5807,#5808);
#5090=AXIS2_PLACEMENT_3D('',#7002,#5809,#5810);
#5091=AXIS2_PLACEMENT_3D('',#7005,#5812,#5813);
#5092=AXIS2_PLACEMENT_3D('',#7006,#5814,#5815);
#5093=AXIS2_PLACEMENT_3D('',#7008,#5816,#5817);
#5094=AXIS2_PLACEMENT_3D('',#7011,#5819,#5820);
#5095=AXIS2_PLACEMENT_3D('',#7012,#5821,#5822);
#5096=AXIS2_PLACEMENT_3D('',#7021,#5827,#5828);
#5097=AXIS2_PLACEMENT_3D('',#7027,#5832,#5833);
#5098=AXIS2_PLACEMENT_3D('',#7033,#5837,#5838);
#5099=AXIS2_PLACEMENT_3D('',#7036,#5841,#5842);
#5100=AXIS2_PLACEMENT_3D('',#7037,#5843,#5844);
#5101=AXIS2_PLACEMENT_3D('',#7038,#5845,#5846);
#5102=AXIS2_PLACEMENT_3D('',#7039,#5847,#5848);
#5103=AXIS2_PLACEMENT_3D('',#7041,#5849,#5850);
#5104=AXIS2_PLACEMENT_3D('',#7044,#5852,#5853);
#5105=AXIS2_PLACEMENT_3D('',#7045,#5854,#5855);
#5106=AXIS2_PLACEMENT_3D('',#7047,#5856,#5857);
#5107=AXIS2_PLACEMENT_3D('',#7050,#5859,#5860);
#5108=AXIS2_PLACEMENT_3D('',#7051,#5861,#5862);
#5109=AXIS2_PLACEMENT_3D('',#7056,#5864,#5865);
#5110=AXIS2_PLACEMENT_3D('',#7060,#5868,#5869);
#5111=AXIS2_PLACEMENT_3D('',#7064,#5871,#5872);
#5112=AXIS2_PLACEMENT_3D('',#7066,#5874,#5875);
#5113=AXIS2_PLACEMENT_3D('',#7072,#5879,#5880);
#5114=AXIS2_PLACEMENT_3D('',#7090,#5890,#5891);
#5115=AXIS2_PLACEMENT_3D('',#7098,#5896,#5897);
#5116=AXIS2_PLACEMENT_3D('',#7106,#5902,#5903);
#5117=AXIS2_PLACEMENT_3D('',#7108,#5904,#5905);
#5118=AXIS2_PLACEMENT_3D('',#7111,#5907,#5908);
#5119=AXIS2_PLACEMENT_3D('',#7112,#5909,#5910);
#5120=AXIS2_PLACEMENT_3D('',#7114,#5911,#5912);
#5121=AXIS2_PLACEMENT_3D('',#7116,#5914,#5915);
#5122=AXIS2_PLACEMENT_3D('',#7119,#5917,#5918);
#5123=AXIS2_PLACEMENT_3D('',#7120,#5919,#5920);
#5124=AXIS2_PLACEMENT_3D('',#7125,#5924,#5925);
#5125=AXIS2_PLACEMENT_3D('',#7137,#5932,#5933);
#5126=AXIS2_PLACEMENT_3D('',#7138,#5934,#5935);
#5127=AXIS2_PLACEMENT_3D('',#7139,#5936,#5937);
#5128=AXIS2_PLACEMENT_3D('',#7140,#5938,#5939);
#5129=AXIS2_PLACEMENT_3D('',#7141,#5940,#5941);
#5130=AXIS2_PLACEMENT_3D('',#7142,#5942,#5943);
#5131=AXIS2_PLACEMENT_3D('',#7143,#5944,#5945);
#5132=AXIS2_PLACEMENT_3D('',#7144,#5946,#5947);
#5133=AXIS2_PLACEMENT_3D('',#7146,#5949,#5950);
#5134=AXIS2_PLACEMENT_3D('',#7147,#5951,#5952);
#5135=AXIS2_PLACEMENT_3D('',#7148,#5953,#5954);
#5136=AXIS2_PLACEMENT_3D('',#7150,#5955,#5956);
#5137=AXIS2_PLACEMENT_3D('',#7153,#5958,#5959);
#5138=AXIS2_PLACEMENT_3D('',#7154,#5960,#5961);
#5139=AXIS2_PLACEMENT_3D('',#7156,#5962,#5963);
#5140=AXIS2_PLACEMENT_3D('',#7159,#5965,#5966);
#5141=AXIS2_PLACEMENT_3D('',#7160,#5967,#5968);
#5142=AXIS2_PLACEMENT_3D('',#7165,#5970,#5971);
#5143=AXIS2_PLACEMENT_3D('',#7167,#5973,#5974);
#5144=AXIS2_PLACEMENT_3D('',#7171,#5976,#5977);
#5145=AXIS2_PLACEMENT_3D('',#7173,#5979,#5980);
#5146=AXIS2_PLACEMENT_3D('',#7193,#5991,#5992);
#5147=AXIS2_PLACEMENT_3D('',#7208,#6001,#6002);
#5148=AXIS2_PLACEMENT_3D('',#7209,#6003,#6004);
#5149=AXIS2_PLACEMENT_3D('',#7210,#6005,#6006);
#5150=AXIS2_PLACEMENT_3D('',#7211,#6007,#6008);
#5151=AXIS2_PLACEMENT_3D('',#7212,#6009,#6010);
#5152=AXIS2_PLACEMENT_3D('',#7216,#6013,#6014);
#5153=AXIS2_PLACEMENT_3D('',#7217,#6015,#6016);
#5154=AXIS2_PLACEMENT_3D('',#7219,#6017,#6018);
#5155=AXIS2_PLACEMENT_3D('',#7220,#6019,#6020);
#5156=AXIS2_PLACEMENT_3D('',#7223,#6022,#6023);
#5157=AXIS2_PLACEMENT_3D('',#7224,#6024,#6025);
#5158=AXIS2_PLACEMENT_3D('',#7225,#6026,#6027);
#5159=AXIS2_PLACEMENT_3D('',#7226,#6028,#6029);
#5160=AXIS2_PLACEMENT_3D('',#7227,#6030,#6031);
#5161=AXIS2_PLACEMENT_3D('',#7231,#6034,#6035);
#5162=AXIS2_PLACEMENT_3D('',#7233,#6037,#6038);
#5163=AXIS2_PLACEMENT_3D('',#7234,#6039,#6040);
#5164=AXIS2_PLACEMENT_3D('',#7235,#6041,#6042);
#5165=AXIS2_PLACEMENT_3D('',#7237,#6043,#6044);
#5166=AXIS2_PLACEMENT_3D('',#7239,#6045,#6046);
#5167=AXIS2_PLACEMENT_3D('',#7240,#6047,#6048);
#5168=AXIS2_PLACEMENT_3D('',#7242,#6049,#6050);
#5169=AXIS2_PLACEMENT_3D('',#7244,#6052,#6053);
#5170=AXIS2_PLACEMENT_3D('',#7246,#6054,#6055);
#5171=AXIS2_PLACEMENT_3D('',#7248,#6056,#6057);
#5172=AXIS2_PLACEMENT_3D('',#7249,#6058,#6059);
#5173=AXIS2_PLACEMENT_3D('',#7252,#6061,#6062);
#5174=AXIS2_PLACEMENT_3D('',#7253,#6063,#6064);
#5175=AXIS2_PLACEMENT_3D('',#7254,#6065,#6066);
#5176=AXIS2_PLACEMENT_3D('',#7256,#6068,#6069);
#5177=AXIS2_PLACEMENT_3D('',#7257,#6070,#6071);
#5178=AXIS2_PLACEMENT_3D('',#7258,#6072,#6073);
#5179=AXIS2_PLACEMENT_3D('',#7274,#6075,#6076);
#5180=AXIS2_PLACEMENT_3D('',#7282,#6077,#6078);
#5181=AXIS2_PLACEMENT_3D('',#7330,#6080,#6081);
#5182=AXIS2_PLACEMENT_3D('',#7378,#6083,#6084);
#5183=AXIS2_PLACEMENT_3D('',#7429,#6086,#6087);
#5184=AXIS2_PLACEMENT_3D('',#7477,#6089,#6090);
#5185=AXIS2_PLACEMENT_3D('',#7525,#6092,#6093);
#5186=AXIS2_PLACEMENT_3D('',#7573,#6095,#6096);
#5187=AXIS2_PLACEMENT_3D('',#7627,#6098,#6099);
#5188=AXIS2_PLACEMENT_3D('',#7675,#6101,#6102);
#5189=AXIS2_PLACEMENT_3D('',#7723,#6104,#6105);
#5190=AXIS2_PLACEMENT_3D('',#7777,#6107,#6108);
#5191=AXIS2_PLACEMENT_3D('',#7825,#6110,#6111);
#5192=AXIS2_PLACEMENT_3D('',#7873,#6113,#6114);
#5193=AXIS2_PLACEMENT_3D('',#7921,#6116,#6117);
#5194=AXIS2_PLACEMENT_3D('',#7975,#6119,#6120);
#5195=AXIS2_PLACEMENT_3D('',#8023,#6122,#6123);
#5196=AXIS2_PLACEMENT_3D('',#8071,#6125,#6126);
#5197=AXIS2_PLACEMENT_3D('',#8125,#6128,#6129);
#5198=AXIS2_PLACEMENT_3D('',#8173,#6131,#6132);
#5199=AXIS2_PLACEMENT_3D('',#8221,#6134,#6135);
#5200=AXIS2_PLACEMENT_3D('',#8275,#6137,#6138);
#5201=AXIS2_PLACEMENT_3D('',#8323,#6140,#6141);
#5202=AXIS2_PLACEMENT_3D('',#8371,#6143,#6144);
#5203=AXIS2_PLACEMENT_3D('',#8419,#6146,#6147);
#5204=AXIS2_PLACEMENT_3D('',#8473,#6149,#6150);
#5205=AXIS2_PLACEMENT_3D('',#8521,#6152,#6153);
#5206=AXIS2_PLACEMENT_3D('',#8569,#6155,#6156);
#5207=AXIS2_PLACEMENT_3D('',#8623,#6158,#6159);
#5208=AXIS2_PLACEMENT_3D('',#8671,#6161,#6162);
#5209=AXIS2_PLACEMENT_3D('',#8719,#6164,#6165);
#5210=AXIS2_PLACEMENT_3D('',#8773,#6167,#6168);
#5211=AXIS2_PLACEMENT_3D('',#8821,#6170,#6171);
#5212=AXIS2_PLACEMENT_3D('',#8869,#6173,#6174);
#5213=AXIS2_PLACEMENT_3D('',#8917,#6176,#6177);
#5214=AXIS2_PLACEMENT_3D('',#8922,#6179,#6180);
#5215=AXIS2_PLACEMENT_3D('',#8970,#6181,#6182);
#5216=AXIS2_PLACEMENT_3D('',#8984,#6184,#6185);
#5217=AXIS2_PLACEMENT_3D('',#8991,#6186,#6187);
#5218=AXIS2_PLACEMENT_3D('',#9016,#6189,#6190);
#5219=AXIS2_PLACEMENT_3D('',#9040,#6192,#6193);
#5220=AXIS2_PLACEMENT_3D('',#9064,#6195,#6196);
#5221=AXIS2_PLACEMENT_3D('',#9089,#6198,#6199);
#5222=AXIS2_PLACEMENT_3D('',#9114,#6201,#6202);
#5223=AXIS2_PLACEMENT_3D('',#9138,#6204,#6205);
#5224=AXIS2_PLACEMENT_3D('',#9163,#6207,#6208);
#5225=AXIS2_PLACEMENT_3D('',#9188,#6210,#6211);
#5226=AXIS2_PLACEMENT_3D('',#9212,#6213,#6214);
#5227=AXIS2_PLACEMENT_3D('',#9237,#6216,#6217);
#5228=AXIS2_PLACEMENT_3D('',#9262,#6219,#6220);
#5229=AXIS2_PLACEMENT_3D('',#9286,#6222,#6223);
#5230=AXIS2_PLACEMENT_3D('',#9310,#6225,#6226);
#5231=AXIS2_PLACEMENT_3D('',#9335,#6228,#6229);
#5232=AXIS2_PLACEMENT_3D('',#9360,#6231,#6232);
#5233=AXIS2_PLACEMENT_3D('',#9384,#6234,#6235);
#5234=AXIS2_PLACEMENT_3D('',#9409,#6237,#6238);
#5235=AXIS2_PLACEMENT_3D('',#9434,#6240,#6241);
#5236=AXIS2_PLACEMENT_3D('',#9458,#6243,#6244);
#5237=AXIS2_PLACEMENT_3D('',#9483,#6246,#6247);
#5238=AXIS2_PLACEMENT_3D('',#9508,#6249,#6250);
#5239=AXIS2_PLACEMENT_3D('',#9532,#6252,#6253);
#5240=AXIS2_PLACEMENT_3D('',#9556,#6255,#6256);
#5241=AXIS2_PLACEMENT_3D('',#9581,#6258,#6259);
#5242=AXIS2_PLACEMENT_3D('',#9606,#6261,#6262);
#5243=AXIS2_PLACEMENT_3D('',#9630,#6264,#6265);
#5244=AXIS2_PLACEMENT_3D('',#9655,#6267,#6268);
#5245=AXIS2_PLACEMENT_3D('',#9680,#6270,#6271);
#5246=AXIS2_PLACEMENT_3D('',#9704,#6273,#6274);
#5247=AXIS2_PLACEMENT_3D('',#9729,#6276,#6277);
#5248=AXIS2_PLACEMENT_3D('',#9753,#6279,#6280);
#5249=AXIS2_PLACEMENT_3D('',#9778,#6282,#6283);
#5250=AXIS2_PLACEMENT_3D('',#10808,#6285,#6286);
#5251=AXIS2_PLACEMENT_3D('',#10810,#6287,#6288);
#5252=AXIS2_PLACEMENT_3D('',#11813,#6289,#6290);
#5253=AXIS2_PLACEMENT_3D('',#11814,#6291,#6292);
#5254=AXIS2_PLACEMENT_3D('',#11815,#6293,#6294);
#5255=AXIS2_PLACEMENT_3D('',#11824,#6299,#6300);
#5256=AXIS2_PLACEMENT_3D('',#11830,#6304,#6305);
#5257=AXIS2_PLACEMENT_3D('',#11836,#6309,#6310);
#5258=AXIS2_PLACEMENT_3D('',#11842,#6314,#6315);
#5259=AXIS2_PLACEMENT_3D('',#11848,#6319,#6320);
#5260=AXIS2_PLACEMENT_3D('',#11851,#6323,#6324);
#5261=AXIS2_PLACEMENT_3D('',#11852,#6325,#6326);
#5262=AXIS2_PLACEMENT_3D('',#11854,#6327,#6328);
#5263=AXIS2_PLACEMENT_3D('',#11855,#6329,#6330);
#5264=AXIS2_PLACEMENT_3D('',#11858,#6332,#6333);
#5265=AXIS2_PLACEMENT_3D('',#11859,#6334,#6335);
#5266=AXIS2_PLACEMENT_3D('',#11860,#6336,#6337);
#5267=AXIS2_PLACEMENT_3D('',#11861,#6338,#6339);
#5268=AXIS2_PLACEMENT_3D('',#11862,#6340,#6341);
#5269=AXIS2_PLACEMENT_3D('',#11867,#6343,#6344);
#5270=AXIS2_PLACEMENT_3D('',#11872,#6345,#6346);
#5271=AXIS2_PLACEMENT_3D('',#11896,#6348,#6349);
#5272=AXIS2_PLACEMENT_3D('',#11919,#6350,#6351);
#5273=AXIS2_PLACEMENT_3D('',#11970,#6353,#6354);
#5274=AXIS2_PLACEMENT_3D('',#12018,#6356,#6357);
#5275=AXIS2_PLACEMENT_3D('',#12069,#6359,#6360);
#5276=AXIS2_PLACEMENT_3D('',#12088,#6362,#6363);
#5277=AXIS2_PLACEMENT_3D('',#12108,#6364,#6365);
#5278=AXIS2_PLACEMENT_3D('',#12120,#6367,#6368);
#5279=AXIS2_PLACEMENT_3D('',#12128,#6369,#6370);
#5280=AXIS2_PLACEMENT_3D('',#12152,#6372,#6373);
#5281=AXIS2_PLACEMENT_3D('',#12177,#6375,#6376);
#5282=AXIS2_PLACEMENT_3D('',#12202,#6378,#6379);
#5283=AXIS2_PLACEMENT_3D('',#12226,#6381,#6382);
#5284=AXIS2_PLACEMENT_3D('',#12237,#6384,#6385);
#5285=AXIS2_PLACEMENT_3D('',#12243,#6386,#6387);
#5286=AXIS2_PLACEMENT_3D('',#12848,#6388,#6389);
#5287=AXIS2_PLACEMENT_3D('',#12861,#6396,#6397);
#5288=AXIS2_PLACEMENT_3D('',#12862,#6398,#6399);
#5289=AXIS2_PLACEMENT_3D('',#12868,#6403,#6404);
#5290=AXIS2_PLACEMENT_3D('',#12872,#6407,#6408);
#5291=AXIS2_PLACEMENT_3D('',#12876,#6411,#6412);
#5292=AXIS2_PLACEMENT_3D('',#12880,#6415,#6416);
#5293=AXIS2_PLACEMENT_3D('',#12884,#6419,#6420);
#5294=AXIS2_PLACEMENT_3D('',#12886,#6422,#6423);
#5295=AXIS2_PLACEMENT_3D('',#12887,#6424,#6425);
#5296=AXIS2_PLACEMENT_3D('',#12888,#6426,#6427);
#5297=AXIS2_PLACEMENT_3D('',#12890,#6428,#6429);
#5298=AXIS2_PLACEMENT_3D('',#12893,#6431,#6432);
#5299=AXIS2_PLACEMENT_3D('',#12894,#6433,#6434);
#5300=AXIS2_PLACEMENT_3D('',#12895,#6435,#6436);
#5301=AXIS2_PLACEMENT_3D('',#12896,#6437,#6438);
#5302=AXIS2_PLACEMENT_3D('',#12897,#6439,#6440);
#5303=AXIS2_PLACEMENT_3D('',#12898,#6441,#6442);
#5304=AXIS2_PLACEMENT_3D('',#12899,#6443,#6444);
#5305=AXIS2_PLACEMENT_3D('',#12900,#6445,#6446);
#5306=AXIS2_PLACEMENT_3D('',#12901,#6447,#6448);
#5307=AXIS2_PLACEMENT_3D('',#12902,#6449,#6450);
#5308=AXIS2_PLACEMENT_3D('',#12903,#6451,#6452);
#5309=AXIS2_PLACEMENT_3D('',#12904,#6453,#6454);
#5310=AXIS2_PLACEMENT_3D('',#12905,#6455,#6456);
#5311=AXIS2_PLACEMENT_3D('',#12906,#6457,#6458);
#5312=AXIS2_PLACEMENT_3D('',#12907,#6459,#6460);
#5313=AXIS2_PLACEMENT_3D('',#12908,#6461,#6462);
#5314=AXIS2_PLACEMENT_3D('',#12909,#6463,#6464);
#5315=AXIS2_PLACEMENT_3D('',#12910,#6465,#6466);
#5316=AXIS2_PLACEMENT_3D('',#12911,#6467,#6468);
#5317=AXIS2_PLACEMENT_3D('',#12912,#6469,#6470);
#5318=AXIS2_PLACEMENT_3D('',#12913,#6471,#6472);
#5319=AXIS2_PLACEMENT_3D('',#12914,#6473,#6474);
#5320=AXIS2_PLACEMENT_3D('',#12915,#6475,#6476);
#5321=AXIS2_PLACEMENT_3D('',#12916,#6477,#6478);
#5322=AXIS2_PLACEMENT_3D('',#12917,#6479,#6480);
#5323=AXIS2_PLACEMENT_3D('',#12918,#6481,#6482);
#5324=AXIS2_PLACEMENT_3D('',#12919,#6483,#6484);
#5325=AXIS2_PLACEMENT_3D('',#12920,#6485,#6486);
#5326=AXIS2_PLACEMENT_3D('',#12921,#6487,#6488);
#5327=AXIS2_PLACEMENT_3D('',#12922,#6489,#6490);
#5328=AXIS2_PLACEMENT_3D('',#12923,#6491,#6492);
#5329=AXIS2_PLACEMENT_3D('',#12924,#6493,#6494);
#5330=AXIS2_PLACEMENT_3D('',#12925,#6495,#6496);
#5331=AXIS2_PLACEMENT_3D('',#12926,#6497,#6498);
#5332=AXIS2_PLACEMENT_3D('',#12927,#6499,#6500);
#5333=AXIS2_PLACEMENT_3D('',#12928,#6501,#6502);
#5334=AXIS2_PLACEMENT_3D('',#12929,#6503,#6504);
#5335=AXIS2_PLACEMENT_3D('',#12930,#6505,#6506);
#5336=AXIS2_PLACEMENT_3D('',#12931,#6507,#6508);
#5337=AXIS2_PLACEMENT_3D('',#12932,#6509,#6510);
#5338=AXIS2_PLACEMENT_3D('',#12933,#6511,#6512);
#5339=AXIS2_PLACEMENT_3D('',#12934,#6513,#6514);
#5340=AXIS2_PLACEMENT_3D('',#12935,#6515,#6516);
#5341=DIRECTION('axis',(0.,0.,1.));
#5342=DIRECTION('refdir',(1.,0.,0.));
#5343=DIRECTION('axis',(0.,0.,1.));
#5344=DIRECTION('refdir',(1.,0.,0.));
#5345=DIRECTION('center_axis',(1.,0.,0.));
#5346=DIRECTION('ref_axis',(0.,0.,-1.));
#5347=DIRECTION('center_axis',(1.,0.,0.));
#5348=DIRECTION('ref_axis',(0.,0.,-1.));
#5349=DIRECTION('',(1.,0.,0.));
#5350=DIRECTION('center_axis',(1.,0.,0.));
#5351=DIRECTION('ref_axis',(0.,0.,-1.));
#5352=DIRECTION('center_axis',(1.,0.,0.));
#5353=DIRECTION('ref_axis',(0.,0.,-1.));
#5354=DIRECTION('center_axis',(-1.,0.,0.));
#5355=DIRECTION('ref_axis',(0.,0.,-1.));
#5356=DIRECTION('center_axis',(1.,0.,0.));
#5357=DIRECTION('ref_axis',(0.,0.,-1.));
#5358=DIRECTION('center_axis',(1.,0.,0.));
#5359=DIRECTION('ref_axis',(0.,0.,-1.));
#5360=DIRECTION('',(1.,0.,0.));
#5361=DIRECTION('center_axis',(1.,0.,0.));
#5362=DIRECTION('ref_axis',(0.,0.,-1.));
#5363=DIRECTION('center_axis',(1.,0.,0.));
#5364=DIRECTION('ref_axis',(0.,0.,-1.));
#5365=DIRECTION('center_axis',(-1.,0.,0.));
#5366=DIRECTION('ref_axis',(0.,0.,-1.));
#5367=DIRECTION('center_axis',(1.,0.,0.));
#5368=DIRECTION('ref_axis',(0.,0.,-1.));
#5369=DIRECTION('center_axis',(1.,0.,0.));
#5370=DIRECTION('ref_axis',(0.,0.,-1.));
#5371=DIRECTION('',(1.,0.,0.));
#5372=DIRECTION('center_axis',(1.,0.,0.));
#5373=DIRECTION('ref_axis',(0.,0.,-1.));
#5374=DIRECTION('center_axis',(1.,0.,0.));
#5375=DIRECTION('ref_axis',(0.,0.,-1.));
#5376=DIRECTION('center_axis',(1.,0.,0.));
#5377=DIRECTION('ref_axis',(0.,0.,-1.));
#5378=DIRECTION('center_axis',(1.,0.,0.));
#5379=DIRECTION('ref_axis',(0.,0.,-1.));
#5380=DIRECTION('',(1.,0.,0.));
#5381=DIRECTION('center_axis',(1.,0.,0.));
#5382=DIRECTION('ref_axis',(0.,0.,-1.));
#5383=DIRECTION('center_axis',(1.,0.,0.));
#5384=DIRECTION('ref_axis',(0.,0.,-1.));
#5385=DIRECTION('center_axis',(1.,0.,0.));
#5386=DIRECTION('ref_axis',(0.,0.,-1.));
#5387=DIRECTION('center_axis',(1.,0.,0.));
#5388=DIRECTION('ref_axis',(0.,0.,-1.));
#5389=DIRECTION('',(1.,0.,0.));
#5390=DIRECTION('center_axis',(1.,0.,0.));
#5391=DIRECTION('ref_axis',(0.,0.,-1.));
#5392=DIRECTION('center_axis',(1.,0.,0.));
#5393=DIRECTION('ref_axis',(0.,0.,-1.));
#5394=DIRECTION('center_axis',(1.,0.,0.));
#5395=DIRECTION('ref_axis',(0.,0.,-1.));
#5396=DIRECTION('center_axis',(1.,0.,0.));
#5397=DIRECTION('ref_axis',(0.,0.,-1.));
#5398=DIRECTION('',(1.,0.,0.));
#5399=DIRECTION('center_axis',(1.,0.,0.));
#5400=DIRECTION('ref_axis',(0.,0.,-1.));
#5401=DIRECTION('center_axis',(1.,0.,0.));
#5402=DIRECTION('ref_axis',(0.,0.,-1.));
#5403=DIRECTION('center_axis',(-1.,0.,0.));
#5404=DIRECTION('ref_axis',(0.,0.,-1.));
#5405=DIRECTION('center_axis',(-1.,0.,0.));
#5406=DIRECTION('ref_axis',(0.,0.,-1.));
#5407=DIRECTION('',(-1.,0.,0.));
#5408=DIRECTION('center_axis',(-1.,0.,0.));
#5409=DIRECTION('ref_axis',(0.,0.,-1.));
#5410=DIRECTION('center_axis',(-1.,0.,0.));
#5411=DIRECTION('ref_axis',(0.,0.,-1.));
#5412=DIRECTION('',(-1.,0.,0.));
#5413=DIRECTION('center_axis',(0.,1.,0.));
#5414=DIRECTION('ref_axis',(-1.,0.,0.));
#5415=DIRECTION('',(1.,0.,0.));
#5416=DIRECTION('',(0.,0.,1.));
#5417=DIRECTION('',(-1.,0.,0.));
#5418=DIRECTION('',(0.,0.,-1.));
#5419=DIRECTION('center_axis',(0.,1.,0.));
#5420=DIRECTION('ref_axis',(-1.,0.,0.));
#5421=DIRECTION('',(1.,0.,0.));
#5422=DIRECTION('',(0.,0.,1.));
#5423=DIRECTION('',(-1.,0.,0.));
#5424=DIRECTION('',(0.,0.,-1.));
#5425=DIRECTION('center_axis',(0.,-1.,0.));
#5426=DIRECTION('ref_axis',(1.,0.,0.));
#5427=DIRECTION('',(-1.,0.,0.));
#5428=DIRECTION('',(0.,0.,1.));
#5429=DIRECTION('',(1.,0.,0.));
#5430=DIRECTION('',(0.,0.,1.));
#5431=DIRECTION('center_axis',(0.,-1.,0.));
#5432=DIRECTION('ref_axis',(1.,0.,0.));
#5433=DIRECTION('',(-1.,0.,0.));
#5434=DIRECTION('',(0.,0.,1.));
#5435=DIRECTION('',(1.,0.,0.));
#5436=DIRECTION('',(0.,0.,1.));
#5437=DIRECTION('center_axis',(-1.,0.,0.));
#5438=DIRECTION('ref_axis',(0.,-1.,0.));
#5439=DIRECTION('',(0.,-1.,0.));
#5440=DIRECTION('',(0.,0.,-1.));
#5441=DIRECTION('',(0.,1.,0.));
#5442=DIRECTION('',(0.,0.,1.));
#5443=DIRECTION('',(0.,-1.,0.));
#5444=DIRECTION('',(0.,-1.,0.));
#5445=DIRECTION('',(0.,0.,1.));
#5446=DIRECTION('',(0.,-1.,0.));
#5447=DIRECTION('',(0.,-1.,0.));
#5448=DIRECTION('',(0.,0.,1.));
#5449=DIRECTION('',(0.,-1.,0.));
#5450=DIRECTION('',(0.,0.,-1.));
#5451=DIRECTION('',(0.,-1.,0.));
#5452=DIRECTION('',(0.,-1.,0.));
#5453=DIRECTION('',(0.,0.,-1.));
#5454=DIRECTION('',(0.,-1.,0.));
#5455=DIRECTION('center_axis',(0.,0.,1.));
#5456=DIRECTION('ref_axis',(1.,0.,0.));
#5457=DIRECTION('',(-1.,0.,0.));
#5458=DIRECTION('',(0.,-1.,0.));
#5459=DIRECTION('center_axis',(0.,0.,1.));
#5460=DIRECTION('ref_axis',(1.,0.,0.));
#5461=DIRECTION('',(0.,-1.,0.));
#5462=DIRECTION('',(1.,0.,0.));
#5463=DIRECTION('center_axis',(1.,0.,0.));
#5464=DIRECTION('ref_axis',(0.,1.,0.));
#5465=DIRECTION('',(0.,0.,1.));
#5466=DIRECTION('',(0.,1.,0.));
#5467=DIRECTION('center_axis',(1.,0.,0.));
#5468=DIRECTION('ref_axis',(0.,1.,0.));
#5469=DIRECTION('',(0.,1.,0.));
#5470=DIRECTION('',(0.,0.,1.));
#5471=DIRECTION('center_axis',(0.,0.,1.));
#5472=DIRECTION('ref_axis',(1.,0.,0.));
#5473=DIRECTION('',(1.,0.,0.));
#5474=DIRECTION('center_axis',(0.,0.,1.));
#5475=DIRECTION('ref_axis',(1.,0.,0.));
#5476=DIRECTION('',(-1.,0.,0.));
#5477=DIRECTION('center_axis',(0.,0.,1.));
#5478=DIRECTION('ref_axis',(1.,0.,0.));
#5479=DIRECTION('',(-1.,0.,0.));
#5480=DIRECTION('',(0.,-1.,0.));
#5481=DIRECTION('center_axis',(0.,0.,1.));
#5482=DIRECTION('ref_axis',(1.,0.,0.));
#5483=DIRECTION('',(0.,-1.,0.));
#5484=DIRECTION('',(1.,0.,0.));
#5485=DIRECTION('center_axis',(1.,0.,0.));
#5486=DIRECTION('ref_axis',(0.,1.,0.));
#5487=DIRECTION('',(0.,0.,1.));
#5488=DIRECTION('',(0.,1.,0.));
#5489=DIRECTION('center_axis',(1.,0.,0.));
#5490=DIRECTION('ref_axis',(0.,1.,0.));
#5491=DIRECTION('',(0.,1.,0.));
#5492=DIRECTION('',(0.,0.,1.));
#5493=DIRECTION('center_axis',(0.,0.,1.));
#5494=DIRECTION('ref_axis',(1.,0.,0.));
#5495=DIRECTION('',(1.,0.,0.));
#5496=DIRECTION('center_axis',(0.,0.,1.));
#5497=DIRECTION('ref_axis',(1.,0.,0.));
#5498=DIRECTION('',(-1.,0.,0.));
#5499=DIRECTION('center_axis',(0.,1.,0.));
#5500=DIRECTION('ref_axis',(-1.,0.,0.));
#5501=DIRECTION('',(-1.,0.,0.));
#5502=DIRECTION('',(0.,0.,1.));
#5503=DIRECTION('',(-1.,0.,0.));
#5504=DIRECTION('center_axis',(0.,0.,1.));
#5505=DIRECTION('ref_axis',(1.,0.,0.));
#5506=DIRECTION('',(1.,0.,0.));
#5507=DIRECTION('',(0.,-1.,0.));
#5508=DIRECTION('center_axis',(0.,-1.,0.));
#5509=DIRECTION('ref_axis',(1.,0.,0.));
#5510=DIRECTION('',(1.,0.,0.));
#5511=DIRECTION('',(0.,0.,1.));
#5512=DIRECTION('center_axis',(-1.,0.,0.));
#5513=DIRECTION('ref_axis',(0.,-1.,0.));
#5514=DIRECTION('',(0.,-1.,0.));
#5515=DIRECTION('center_axis',(0.,0.,1.));
#5516=DIRECTION('ref_axis',(1.,0.,0.));
#5517=DIRECTION('axis',(0.,0.,1.));
#5518=DIRECTION('refdir',(1.,0.,0.));
#5519=DIRECTION('center_axis',(1.,0.,0.));
#5520=DIRECTION('ref_axis',(0.,0.,-1.));
#5521=DIRECTION('center_axis',(1.,0.,0.));
#5522=DIRECTION('ref_axis',(0.,0.,-1.));
#5523=DIRECTION('',(1.,0.,0.));
#5524=DIRECTION('center_axis',(1.,0.,0.));
#5525=DIRECTION('ref_axis',(0.,0.,-1.));
#5526=DIRECTION('center_axis',(1.,0.,0.));
#5527=DIRECTION('ref_axis',(0.,0.,-1.));
#5528=DIRECTION('center_axis',(1.,0.,0.));
#5529=DIRECTION('ref_axis',(0.,0.,-1.));
#5530=DIRECTION('center_axis',(1.,0.,0.));
#5531=DIRECTION('ref_axis',(0.,0.,-1.));
#5532=DIRECTION('',(1.,0.,0.));
#5533=DIRECTION('center_axis',(1.,0.,0.));
#5534=DIRECTION('ref_axis',(0.,0.,-1.));
#5535=DIRECTION('center_axis',(1.,0.,0.));
#5536=DIRECTION('ref_axis',(0.,0.,-1.));
#5537=DIRECTION('center_axis',(1.,0.,0.));
#5538=DIRECTION('ref_axis',(0.,0.,-1.));
#5539=DIRECTION('center_axis',(1.,0.,0.));
#5540=DIRECTION('ref_axis',(0.,0.,-1.));
#5541=DIRECTION('',(1.,0.,0.));
#5542=DIRECTION('center_axis',(1.,0.,0.));
#5543=DIRECTION('ref_axis',(0.,0.,-1.));
#5544=DIRECTION('center_axis',(1.,0.,0.));
#5545=DIRECTION('ref_axis',(0.,0.,-1.));
#5546=DIRECTION('center_axis',(1.,0.,0.));
#5547=DIRECTION('ref_axis',(0.,0.,-1.));
#5548=DIRECTION('center_axis',(1.,0.,0.));
#5549=DIRECTION('ref_axis',(0.,0.,-1.));
#5550=DIRECTION('',(1.,0.,0.));
#5551=DIRECTION('center_axis',(1.,0.,0.));
#5552=DIRECTION('ref_axis',(0.,0.,-1.));
#5553=DIRECTION('center_axis',(1.,0.,0.));
#5554=DIRECTION('ref_axis',(0.,0.,-1.));
#5555=DIRECTION('center_axis',(-1.,0.,0.));
#5556=DIRECTION('ref_axis',(0.,0.,-1.));
#5557=DIRECTION('center_axis',(-1.,0.,0.));
#5558=DIRECTION('ref_axis',(0.,0.,-1.));
#5559=DIRECTION('',(-1.,0.,0.));
#5560=DIRECTION('center_axis',(1.,0.,0.));
#5561=DIRECTION('ref_axis',(0.,0.,-1.));
#5562=DIRECTION('center_axis',(-1.,0.,0.));
#5563=DIRECTION('ref_axis',(0.,0.,-1.));
#5564=DIRECTION('center_axis',(-1.,0.,0.));
#5565=DIRECTION('ref_axis',(0.,0.,-1.));
#5566=DIRECTION('',(-1.,0.,0.));
#5567=DIRECTION('center_axis',(1.,0.,0.));
#5568=DIRECTION('ref_axis',(0.,0.,-1.));
#5569=DIRECTION('center_axis',(0.,1.,0.));
#5570=DIRECTION('ref_axis',(-1.,0.,0.));
#5571=DIRECTION('',(1.,0.,0.));
#5572=DIRECTION('',(0.,0.,1.));
#5573=DIRECTION('',(-1.,0.,0.));
#5574=DIRECTION('',(0.,0.,-1.));
#5575=DIRECTION('center_axis',(0.,1.,0.));
#5576=DIRECTION('ref_axis',(-1.,0.,0.));
#5577=DIRECTION('',(1.,0.,0.));
#5578=DIRECTION('',(0.,0.,1.));
#5579=DIRECTION('',(-1.,0.,0.));
#5580=DIRECTION('',(0.,0.,-1.));
#5581=DIRECTION('center_axis',(0.,-1.,0.));
#5582=DIRECTION('ref_axis',(1.,0.,0.));
#5583=DIRECTION('',(-1.,0.,0.));
#5584=DIRECTION('',(0.,0.,1.));
#5585=DIRECTION('',(1.,0.,0.));
#5586=DIRECTION('',(0.,0.,1.));
#5587=DIRECTION('center_axis',(0.,-1.,0.));
#5588=DIRECTION('ref_axis',(1.,0.,0.));
#5589=DIRECTION('',(-1.,0.,0.));
#5590=DIRECTION('',(0.,0.,1.));
#5591=DIRECTION('',(1.,0.,0.));
#5592=DIRECTION('',(0.,0.,1.));
#5593=DIRECTION('center_axis',(-1.,0.,0.));
#5594=DIRECTION('ref_axis',(0.,-1.,0.));
#5595=DIRECTION('',(0.,-1.,0.));
#5596=DIRECTION('',(0.,0.,-1.));
#5597=DIRECTION('',(0.,1.,0.));
#5598=DIRECTION('',(0.,0.,1.));
#5599=DIRECTION('',(0.,-1.,0.));
#5600=DIRECTION('',(0.,-1.,0.));
#5601=DIRECTION('',(0.,0.,1.));
#5602=DIRECTION('',(0.,-1.,0.));
#5603=DIRECTION('',(0.,-1.,0.));
#5604=DIRECTION('',(0.,0.,1.));
#5605=DIRECTION('',(0.,-1.,0.));
#5606=DIRECTION('',(0.,0.,-1.));
#5607=DIRECTION('',(0.,-1.,0.));
#5608=DIRECTION('',(0.,-1.,0.));
#5609=DIRECTION('',(0.,0.,-1.));
#5610=DIRECTION('',(0.,-1.,0.));
#5611=DIRECTION('center_axis',(0.,0.,1.));
#5612=DIRECTION('ref_axis',(1.,0.,0.));
#5613=DIRECTION('',(-1.,0.,0.));
#5614=DIRECTION('',(0.,-1.,0.));
#5615=DIRECTION('center_axis',(0.,0.,1.));
#5616=DIRECTION('ref_axis',(1.,0.,0.));
#5617=DIRECTION('',(0.,-1.,0.));
#5618=DIRECTION('',(1.,0.,0.));
#5619=DIRECTION('center_axis',(1.,0.,0.));
#5620=DIRECTION('ref_axis',(0.,1.,0.));
#5621=DIRECTION('',(0.,0.,1.));
#5622=DIRECTION('',(0.,1.,0.));
#5623=DIRECTION('center_axis',(1.,0.,0.));
#5624=DIRECTION('ref_axis',(0.,1.,0.));
#5625=DIRECTION('',(0.,1.,0.));
#5626=DIRECTION('',(0.,0.,1.));
#5627=DIRECTION('center_axis',(0.,0.,1.));
#5628=DIRECTION('ref_axis',(1.,0.,0.));
#5629=DIRECTION('',(1.,0.,0.));
#5630=DIRECTION('center_axis',(0.,0.,1.));
#5631=DIRECTION('ref_axis',(1.,0.,0.));
#5632=DIRECTION('',(-1.,0.,0.));
#5633=DIRECTION('center_axis',(0.,0.,1.));
#5634=DIRECTION('ref_axis',(1.,0.,0.));
#5635=DIRECTION('',(-1.,0.,0.));
#5636=DIRECTION('',(0.,-1.,0.));
#5637=DIRECTION('center_axis',(0.,0.,1.));
#5638=DIRECTION('ref_axis',(1.,0.,0.));
#5639=DIRECTION('',(0.,-1.,0.));
#5640=DIRECTION('',(1.,0.,0.));
#5641=DIRECTION('center_axis',(1.,0.,0.));
#5642=DIRECTION('ref_axis',(0.,1.,0.));
#5643=DIRECTION('',(0.,0.,1.));
#5644=DIRECTION('',(0.,1.,0.));
#5645=DIRECTION('center_axis',(1.,0.,0.));
#5646=DIRECTION('ref_axis',(0.,1.,0.));
#5647=DIRECTION('',(0.,1.,0.));
#5648=DIRECTION('',(0.,0.,1.));
#5649=DIRECTION('center_axis',(0.,0.,1.));
#5650=DIRECTION('ref_axis',(1.,0.,0.));
#5651=DIRECTION('',(1.,0.,0.));
#5652=DIRECTION('center_axis',(0.,0.,1.));
#5653=DIRECTION('ref_axis',(1.,0.,0.));
#5654=DIRECTION('',(-1.,0.,0.));
#5655=DIRECTION('center_axis',(0.,1.,0.));
#5656=DIRECTION('ref_axis',(-1.,0.,0.));
#5657=DIRECTION('',(-1.,0.,0.));
#5658=DIRECTION('',(0.,0.,1.));
#5659=DIRECTION('',(-1.,0.,0.));
#5660=DIRECTION('center_axis',(0.,0.,1.));
#5661=DIRECTION('ref_axis',(1.,0.,0.));
#5662=DIRECTION('',(1.,0.,0.));
#5663=DIRECTION('',(0.,-1.,0.));
#5664=DIRECTION('center_axis',(0.,-1.,0.));
#5665=DIRECTION('ref_axis',(1.,0.,0.));
#5666=DIRECTION('',(1.,0.,0.));
#5667=DIRECTION('',(0.,0.,1.));
#5668=DIRECTION('center_axis',(-1.,0.,0.));
#5669=DIRECTION('ref_axis',(0.,-1.,0.));
#5670=DIRECTION('',(0.,-1.,0.));
#5671=DIRECTION('center_axis',(0.,0.,1.));
#5672=DIRECTION('ref_axis',(1.,0.,0.));
#5673=DIRECTION('axis',(0.,0.,1.));
#5674=DIRECTION('refdir',(1.,0.,0.));
#5675=DIRECTION('center_axis',(0.,-1.,0.));
#5676=DIRECTION('ref_axis',(1.,0.,0.));
#5677=DIRECTION('',(-1.,0.,0.));
#5678=DIRECTION('',(0.,0.,1.));
#5679=DIRECTION('',(1.,0.,0.));
#5680=DIRECTION('',(0.,0.,-1.));
#5681=DIRECTION('center_axis',(0.,1.,0.));
#5682=DIRECTION('ref_axis',(-1.,0.,0.));
#5683=DIRECTION('',(1.,0.,0.));
#5684=DIRECTION('',(0.,0.,1.));
#5685=DIRECTION('',(-1.,0.,0.));
#5686=DIRECTION('',(0.,0.,-1.));
#5687=DIRECTION('center_axis',(0.,0.,1.));
#5688=DIRECTION('ref_axis',(1.,0.,0.));
#5689=DIRECTION('',(0.,1.,0.));
#5690=DIRECTION('',(0.,-1.,0.));
#5691=DIRECTION('center_axis',(1.,0.,0.));
#5692=DIRECTION('ref_axis',(0.,1.,0.));
#5693=DIRECTION('',(0.,1.,0.));
#5694=DIRECTION('',(0.,0.,1.));
#5695=DIRECTION('',(0.,1.,0.));
#5696=DIRECTION('',(0.,0.,1.));
#5697=DIRECTION('',(0.,1.,0.));
#5698=DIRECTION('center_axis',(0.,0.,1.));
#5699=DIRECTION('ref_axis',(1.,0.,0.));
#5700=DIRECTION('',(0.,-1.,0.));
#5701=DIRECTION('',(1.,0.,0.));
#5702=DIRECTION('center_axis',(0.,1.,0.));
#5703=DIRECTION('ref_axis',(-1.,0.,0.));
#5704=DIRECTION('',(-1.,0.,0.));
#5705=DIRECTION('',(0.,0.,1.));
#5706=DIRECTION('',(-1.,0.,0.));
#5707=DIRECTION('center_axis',(0.,-1.,0.));
#5708=DIRECTION('ref_axis',(1.,0.,0.));
#5709=DIRECTION('',(1.,0.,0.));
#5710=DIRECTION('',(0.,0.,1.));
#5711=DIRECTION('center_axis',(-1.,0.,0.));
#5712=DIRECTION('ref_axis',(0.,-1.,0.));
#5713=DIRECTION('',(0.,-1.,0.));
#5714=DIRECTION('',(0.,-1.,0.));
#5715=DIRECTION('center_axis',(0.,0.,1.));
#5716=DIRECTION('ref_axis',(1.,0.,0.));
#5717=DIRECTION('center_axis',(0.,0.,1.));
#5718=DIRECTION('ref_axis',(1.,0.,0.));
#5719=DIRECTION('axis',(0.,0.,1.));
#5720=DIRECTION('refdir',(1.,0.,0.));
#5721=DIRECTION('center_axis',(0.,1.,0.));
#5722=DIRECTION('ref_axis',(-1.,0.,0.));
#5723=DIRECTION('',(-1.,0.,0.));
#5724=DIRECTION('',(0.,0.,1.));
#5725=DIRECTION('',(-1.,0.,0.));
#5726=DIRECTION('',(0.,0.,1.));
#5727=DIRECTION('center_axis',(1.,0.,0.));
#5728=DIRECTION('ref_axis',(0.,1.,0.));
#5729=DIRECTION('',(0.,1.,0.));
#5730=DIRECTION('',(0.,1.,0.));
#5731=DIRECTION('',(0.,0.,1.));
#5732=DIRECTION('center_axis',(0.,-1.,0.));
#5733=DIRECTION('ref_axis',(1.,0.,0.));
#5734=DIRECTION('',(1.,0.,0.));
#5735=DIRECTION('',(1.,0.,0.));
#5736=DIRECTION('',(0.,0.,1.));
#5737=DIRECTION('center_axis',(-1.,0.,0.));
#5738=DIRECTION('ref_axis',(0.,-1.,0.));
#5739=DIRECTION('',(0.,-1.,0.));
#5740=DIRECTION('',(0.,-1.,0.));
#5741=DIRECTION('center_axis',(0.,0.,1.));
#5742=DIRECTION('ref_axis',(1.,0.,0.));
#5743=DIRECTION('center_axis',(0.,0.,1.));
#5744=DIRECTION('ref_axis',(1.,0.,0.));
#5745=DIRECTION('axis',(0.,0.,1.));
#5746=DIRECTION('refdir',(1.,0.,0.));
#5747=DIRECTION('center_axis',(0.,1.,0.));
#5748=DIRECTION('ref_axis',(-1.,0.,0.));
#5749=DIRECTION('',(-1.,0.,0.));
#5750=DIRECTION('',(0.,0.,1.));
#5751=DIRECTION('',(1.,0.,0.));
#5752=DIRECTION('',(0.,0.,1.));
#5753=DIRECTION('center_axis',(1.,0.,0.));
#5754=DIRECTION('ref_axis',(0.,1.,0.));
#5755=DIRECTION('',(0.,1.,0.));
#5756=DIRECTION('',(0.,0.,-1.));
#5757=DIRECTION('',(0.,-1.,0.));
#5758=DIRECTION('center_axis',(-1.,0.,0.));
#5759=DIRECTION('ref_axis',(0.,-1.,0.));
#5760=DIRECTION('',(0.,-1.,0.));
#5761=DIRECTION('',(0.,0.,1.));
#5762=DIRECTION('',(0.,-1.,0.));
#5763=DIRECTION('center_axis',(0.,-1.,0.));
#5764=DIRECTION('ref_axis',(1.,0.,0.));
#5765=DIRECTION('',(1.,0.,0.));
#5766=DIRECTION('',(0.,0.,1.));
#5767=DIRECTION('',(1.,0.,0.));
#5768=DIRECTION('center_axis',(0.,1.,0.));
#5769=DIRECTION('ref_axis',(-1.,0.,0.));
#5770=DIRECTION('',(-1.,0.,0.));
#5771=DIRECTION('',(-1.,0.,0.));
#5772=DIRECTION('',(0.,0.,1.));
#5773=DIRECTION('center_axis',(1.,0.,0.));
#5774=DIRECTION('ref_axis',(0.,1.,0.));
#5775=DIRECTION('',(0.,1.,0.));
#5776=DIRECTION('',(0.,1.,0.));
#5777=DIRECTION('center_axis',(0.,0.,1.));
#5778=DIRECTION('ref_axis',(1.,0.,0.));
#5779=DIRECTION('center_axis',(0.,0.,1.));
#5780=DIRECTION('ref_axis',(1.,0.,0.));
#5781=DIRECTION('axis',(0.,0.,1.));
#5782=DIRECTION('refdir',(1.,0.,0.));
#5783=DIRECTION('center_axis',(0.,0.,-1.));
#5784=DIRECTION('ref_axis',(1.,0.,0.));
#5785=DIRECTION('',(1.,0.,0.));
#5786=DIRECTION('',(0.,-1.,0.));
#5787=DIRECTION('',(-1.,0.,0.));
#5788=DIRECTION('',(0.,-1.,0.));
#5789=DIRECTION('center_axis',(0.,-1.,0.));
#5790=DIRECTION('ref_axis',(0.,0.,-1.));
#5791=DIRECTION('center_axis',(0.,-1.,0.));
#5792=DIRECTION('ref_axis',(0.,0.,-1.));
#5793=DIRECTION('',(0.,-1.,0.));
#5794=DIRECTION('center_axis',(0.,1.,0.));
#5795=DIRECTION('ref_axis',(0.,0.,-1.));
#5796=DIRECTION('center_axis',(0.,0.,1.));
#5797=DIRECTION('ref_axis',(-1.,0.,0.));
#5798=DIRECTION('',(-1.,0.,0.));
#5799=DIRECTION('',(0.,-1.,0.));
#5800=DIRECTION('',(1.,0.,0.));
#5801=DIRECTION('center_axis',(0.,-1.,0.));
#5802=DIRECTION('ref_axis',(0.,0.,1.));
#5803=DIRECTION('center_axis',(0.,-1.,0.));
#5804=DIRECTION('ref_axis',(0.,0.,1.));
#5805=DIRECTION('center_axis',(0.,1.,0.));
#5806=DIRECTION('ref_axis',(0.,0.,1.));
#5807=DIRECTION('center_axis',(0.,-1.,0.));
#5808=DIRECTION('ref_axis',(1.,0.,0.));
#5809=DIRECTION('center_axis',(0.,-1.,0.));
#5810=DIRECTION('ref_axis',(1.,0.,0.));
#5811=DIRECTION('',(0.,-1.,0.));
#5812=DIRECTION('center_axis',(0.,1.,0.));
#5813=DIRECTION('ref_axis',(1.,0.,0.));
#5814=DIRECTION('center_axis',(0.,-1.,0.));
#5815=DIRECTION('ref_axis',(1.,0.,0.));
#5816=DIRECTION('center_axis',(0.,-1.,0.));
#5817=DIRECTION('ref_axis',(1.,0.,0.));
#5818=DIRECTION('',(0.,-1.,0.));
#5819=DIRECTION('center_axis',(0.,1.,0.));
#5820=DIRECTION('ref_axis',(1.,0.,0.));
#5821=DIRECTION('center_axis',(0.,1.,0.));
#5822=DIRECTION('ref_axis',(-1.,0.,0.));
#5823=DIRECTION('',(-1.,0.,0.));
#5824=DIRECTION('',(0.,0.,1.));
#5825=DIRECTION('',(-1.,0.,0.));
#5826=DIRECTION('',(0.,0.,1.));
#5827=DIRECTION('center_axis',(1.,0.,0.));
#5828=DIRECTION('ref_axis',(0.,1.,0.));
#5829=DIRECTION('',(0.,1.,0.));
#5830=DIRECTION('',(0.,1.,0.));
#5831=DIRECTION('',(0.,0.,1.));
#5832=DIRECTION('center_axis',(0.,-1.,0.));
#5833=DIRECTION('ref_axis',(1.,0.,0.));
#5834=DIRECTION('',(1.,0.,0.));
#5835=DIRECTION('',(1.,0.,0.));
#5836=DIRECTION('',(0.,0.,1.));
#5837=DIRECTION('center_axis',(-1.,0.,0.));
#5838=DIRECTION('ref_axis',(0.,-1.,0.));
#5839=DIRECTION('',(0.,-1.,0.));
#5840=DIRECTION('',(0.,-1.,0.));
#5841=DIRECTION('center_axis',(0.,0.,1.));
#5842=DIRECTION('ref_axis',(1.,0.,0.));
#5843=DIRECTION('center_axis',(0.,0.,1.));
#5844=DIRECTION('ref_axis',(1.,0.,0.));
#5845=DIRECTION('axis',(0.,0.,1.));
#5846=DIRECTION('refdir',(1.,0.,0.));
#5847=DIRECTION('center_axis',(1.,0.,0.));
#5848=DIRECTION('ref_axis',(0.,0.,-1.));
#5849=DIRECTION('center_axis',(1.,0.,0.));
#5850=DIRECTION('ref_axis',(0.,0.,-1.));
#5851=DIRECTION('',(1.,0.,0.));
#5852=DIRECTION('center_axis',(-1.,0.,0.));
#5853=DIRECTION('ref_axis',(0.,0.,-1.));
#5854=DIRECTION('center_axis',(1.,0.,0.));
#5855=DIRECTION('ref_axis',(0.,0.,-1.));
#5856=DIRECTION('center_axis',(1.,0.,0.));
#5857=DIRECTION('ref_axis',(0.,0.,-1.));
#5858=DIRECTION('',(1.,0.,0.));
#5859=DIRECTION('center_axis',(-1.,0.,0.));
#5860=DIRECTION('ref_axis',(0.,0.,-1.));
#5861=DIRECTION('center_axis',(0.,0.,1.));
#5862=DIRECTION('ref_axis',(1.,0.,0.));
#5863=DIRECTION('',(0.,-1.,0.));
#5864=DIRECTION('center_axis',(0.,0.,1.));
#5865=DIRECTION('ref_axis',(1.,0.,0.));
#5866=DIRECTION('',(0.,1.,0.));
#5867=DIRECTION('',(1.,0.,0.));
#5868=DIRECTION('center_axis',(0.,0.,1.));
#5869=DIRECTION('ref_axis',(1.,0.,0.));
#5870=DIRECTION('',(0.,0.,1.));
#5871=DIRECTION('center_axis',(0.,0.,1.));
#5872=DIRECTION('ref_axis',(1.,0.,0.));
#5873=DIRECTION('',(0.,0.,-1.));
#5874=DIRECTION('center_axis',(0.,0.,1.));
#5875=DIRECTION('ref_axis',(1.,0.,0.));
#5876=DIRECTION('',(0.,1.,0.));
#5877=DIRECTION('',(-1.,0.,0.));
#5878=DIRECTION('',(0.,-1.,0.));
#5879=DIRECTION('center_axis',(1.,0.,0.));
#5880=DIRECTION('ref_axis',(0.,1.,0.));
#5881=DIRECTION('',(0.,0.,1.));
#5882=DIRECTION('',(0.,1.,0.));
#5883=DIRECTION('',(0.,0.,-1.));
#5884=DIRECTION('',(0.,1.,0.));
#5885=DIRECTION('',(0.,0.,1.));
#5886=DIRECTION('',(0.,1.,0.));
#5887=DIRECTION('',(0.,0.,-1.));
#5888=DIRECTION('',(0.,-1.,0.));
#5889=DIRECTION('',(0.,0.,1.));
#5890=DIRECTION('center_axis',(0.,-1.,0.));
#5891=DIRECTION('ref_axis',(1.,0.,0.));
#5892=DIRECTION('',(0.,0.,1.));
#5893=DIRECTION('',(1.,0.,0.));
#5894=DIRECTION('',(0.,0.,1.));
#5895=DIRECTION('',(1.,0.,0.));
#5896=DIRECTION('center_axis',(0.,-1.,0.));
#5897=DIRECTION('ref_axis',(1.,0.,0.));
#5898=DIRECTION('',(-1.,0.,0.));
#5899=DIRECTION('',(0.,0.,1.));
#5900=DIRECTION('',(1.,0.,0.));
#5901=DIRECTION('',(0.,0.,1.));
#5902=DIRECTION('center_axis',(0.,0.,1.));
#5903=DIRECTION('ref_axis',(1.,0.,0.));
#5904=DIRECTION('center_axis',(0.,0.,1.));
#5905=DIRECTION('ref_axis',(1.,0.,0.));
#5906=DIRECTION('',(0.,1.,0.));
#5907=DIRECTION('center_axis',(0.,0.,-1.));
#5908=DIRECTION('ref_axis',(1.,0.,0.));
#5909=DIRECTION('center_axis',(0.,0.,1.));
#5910=DIRECTION('ref_axis',(-0.25881904510252,-0.965925826289069,0.));
#5911=DIRECTION('center_axis',(0.,0.,1.));
#5912=DIRECTION('ref_axis',(1.,0.,0.));
#5913=DIRECTION('',(0.,0.,1.));
#5914=DIRECTION('center_axis',(0.,0.,1.));
#5915=DIRECTION('ref_axis',(-0.213200716355611,-0.977008420918394,0.));
#5916=DIRECTION('',(0.,0.,-1.));
#5917=DIRECTION('center_axis',(0.,0.,-1.));
#5918=DIRECTION('ref_axis',(1.,0.,0.));
#5919=DIRECTION('center_axis',(0.,0.,1.));
#5920=DIRECTION('ref_axis',(1.,0.,0.));
#5921=DIRECTION('',(-1.,0.,0.));
#5922=DIRECTION('',(0.,-1.,0.));
#5923=DIRECTION('',(0.,-1.,0.));
#5924=DIRECTION('center_axis',(-1.,0.,0.));
#5925=DIRECTION('ref_axis',(0.,-1.,0.));
#5926=DIRECTION('',(0.,0.,1.));
#5927=DIRECTION('',(0.,-1.,0.));
#5928=DIRECTION('',(0.,0.,1.));
#5929=DIRECTION('',(0.,-1.,0.));
#5930=DIRECTION('',(0.,0.,-1.));
#5931=DIRECTION('',(0.,-1.,0.));
#5932=DIRECTION('center_axis',(0.,0.,1.));
#5933=DIRECTION('ref_axis',(-0.213200716355611,-0.977008420918394,0.));
#5934=DIRECTION('center_axis',(0.,0.,-1.));
#5935=DIRECTION('ref_axis',(1.,0.,0.));
#5936=DIRECTION('center_axis',(0.,0.,-1.));
#5937=DIRECTION('ref_axis',(1.,0.,0.));
#5938=DIRECTION('center_axis',(0.,0.,1.));
#5939=DIRECTION('ref_axis',(-0.25881904510252,-0.965925826289069,0.));
#5940=DIRECTION('center_axis',(0.,0.,1.));
#5941=DIRECTION('ref_axis',(1.,0.,0.));
#5942=DIRECTION('center_axis',(0.,0.,1.));
#5943=DIRECTION('ref_axis',(1.,0.,0.));
#5944=DIRECTION('center_axis',(0.,0.,1.));
#5945=DIRECTION('ref_axis',(1.,0.,0.));
#5946=DIRECTION('center_axis',(0.,1.,0.));
#5947=DIRECTION('ref_axis',(-1.,0.,0.));
#5948=DIRECTION('',(-1.,0.,0.));
#5949=DIRECTION('center_axis',(0.,0.,1.));
#5950=DIRECTION('ref_axis',(1.,0.,0.));
#5951=DIRECTION('axis',(0.,0.,1.));
#5952=DIRECTION('refdir',(1.,0.,0.));
#5953=DIRECTION('center_axis',(0.,-1.,0.));
#5954=DIRECTION('ref_axis',(1.,0.,0.));
#5955=DIRECTION('center_axis',(0.,-1.,0.));
#5956=DIRECTION('ref_axis',(1.,0.,0.));
#5957=DIRECTION('',(0.,-1.,0.));
#5958=DIRECTION('center_axis',(0.,1.,0.));
#5959=DIRECTION('ref_axis',(1.,0.,0.));
#5960=DIRECTION('center_axis',(0.,-1.,0.));
#5961=DIRECTION('ref_axis',(1.,0.,0.));
#5962=DIRECTION('center_axis',(0.,-1.,0.));
#5963=DIRECTION('ref_axis',(1.,0.,0.));
#5964=DIRECTION('',(0.,-1.,0.));
#5965=DIRECTION('center_axis',(0.,1.,0.));
#5966=DIRECTION('ref_axis',(1.,0.,0.));
#5967=DIRECTION('center_axis',(0.,0.,1.));
#5968=DIRECTION('ref_axis',(1.,0.,0.));
#5969=DIRECTION('',(-1.,0.,0.));
#5970=DIRECTION('center_axis',(0.,0.,1.));
#5971=DIRECTION('ref_axis',(1.,0.,0.));
#5972=DIRECTION('',(0.,1.,0.));
#5973=DIRECTION('center_axis',(0.,0.,1.));
#5974=DIRECTION('ref_axis',(1.,0.,0.));
#5975=DIRECTION('',(0.,0.,-1.));
#5976=DIRECTION('center_axis',(0.,0.,-1.));
#5977=DIRECTION('ref_axis',(1.,0.,0.));
#5978=DIRECTION('',(0.,0.,1.));
#5979=DIRECTION('center_axis',(0.,-1.,0.));
#5980=DIRECTION('ref_axis',(1.,0.,0.));
#5981=DIRECTION('',(0.,0.,1.));
#5982=DIRECTION('',(1.,0.,0.));
#5983=DIRECTION('',(0.,0.,-1.));
#5984=DIRECTION('',(-1.,0.,0.));
#5985=DIRECTION('',(0.,0.,1.));
#5986=DIRECTION('',(1.,0.,0.));
#5987=DIRECTION('',(0.,0.,-1.));
#5988=DIRECTION('',(1.,0.,0.));
#5989=DIRECTION('',(0.,0.,1.));
#5990=DIRECTION('',(1.,0.,0.));
#5991=DIRECTION('center_axis',(-1.,0.,0.));
#5992=DIRECTION('ref_axis',(0.,-1.,0.));
#5993=DIRECTION('',(0.,-1.,0.));
#5994=DIRECTION('',(0.,0.,1.));
#5995=DIRECTION('',(0.,-1.,0.));
#5996=DIRECTION('',(0.,0.,1.));
#5997=DIRECTION('',(0.,-1.,0.));
#5998=DIRECTION('',(0.,1.,0.));
#5999=DIRECTION('',(0.,0.,1.));
#6000=DIRECTION('',(0.,-1.,0.));
#6001=DIRECTION('center_axis',(0.,0.,1.));
#6002=DIRECTION('ref_axis',(1.,0.,0.));
#6003=DIRECTION('center_axis',(0.,0.,1.));
#6004=DIRECTION('ref_axis',(1.,0.,0.));
#6005=DIRECTION('center_axis',(0.,0.,1.));
#6006=DIRECTION('ref_axis',(1.,0.,0.));
#6007=DIRECTION('center_axis',(0.,0.,1.));
#6008=DIRECTION('ref_axis',(1.,0.,0.));
#6009=DIRECTION('center_axis',(0.,0.,1.));
#6010=DIRECTION('ref_axis',(1.,0.,0.));
#6011=DIRECTION('',(-1.,0.,0.));
#6012=DIRECTION('',(0.,1.,0.));
#6013=DIRECTION('center_axis',(0.,0.,1.));
#6014=DIRECTION('ref_axis',(1.,0.,0.));
#6015=DIRECTION('center_axis',(0.,0.,1.));
#6016=DIRECTION('ref_axis',(1.,0.,0.));
#6017=DIRECTION('center_axis',(0.,0.,-1.));
#6018=DIRECTION('ref_axis',(1.,0.,0.));
#6019=DIRECTION('center_axis',(0.,0.,1.));
#6020=DIRECTION('ref_axis',(1.,0.,0.));
#6021=DIRECTION('',(0.,0.,-1.));
#6022=DIRECTION('center_axis',(0.,0.,-1.));
#6023=DIRECTION('ref_axis',(1.,0.,0.));
#6024=DIRECTION('center_axis',(0.,0.,1.));
#6025=DIRECTION('ref_axis',(-0.758601839724033,-0.651554486414845,0.));
#6026=DIRECTION('center_axis',(0.,0.,1.));
#6027=DIRECTION('ref_axis',(1.,0.,0.));
#6028=DIRECTION('center_axis',(0.,0.,1.));
#6029=DIRECTION('ref_axis',(1.,0.,0.));
#6030=DIRECTION('center_axis',(0.,1.,0.));
#6031=DIRECTION('ref_axis',(-1.,0.,0.));
#6032=DIRECTION('',(-1.,0.,0.));
#6033=DIRECTION('',(0.,0.,1.));
#6034=DIRECTION('center_axis',(1.,0.,0.));
#6035=DIRECTION('ref_axis',(0.,1.,0.));
#6036=DIRECTION('',(0.,1.,0.));
#6037=DIRECTION('center_axis',(0.,0.,1.));
#6038=DIRECTION('ref_axis',(1.,0.,0.));
#6039=DIRECTION('axis',(0.,0.,1.));
#6040=DIRECTION('refdir',(1.,0.,0.));
#6041=DIRECTION('center_axis',(0.,0.,1.));
#6042=DIRECTION('ref_axis',(1.,0.,0.));
#6043=DIRECTION('center_axis',(0.,0.,1.));
#6044=DIRECTION('ref_axis',(1.,0.,0.));
#6045=DIRECTION('center_axis',(0.,0.,-1.));
#6046=DIRECTION('ref_axis',(1.,0.,0.));
#6047=DIRECTION('center_axis',(0.,0.,1.));
#6048=DIRECTION('ref_axis',(1.,0.,0.));
#6049=DIRECTION('center_axis',(0.,0.,1.));
#6050=DIRECTION('ref_axis',(1.,0.,0.));
#6051=DIRECTION('',(0.,0.,-1.));
#6052=DIRECTION('center_axis',(0.,0.,1.));
#6053=DIRECTION('ref_axis',(1.,0.,0.));
#6054=DIRECTION('center_axis',(0.,0.,1.));
#6055=DIRECTION('ref_axis',(1.,0.,0.));
#6056=DIRECTION('center_axis',(0.,0.,1.));
#6057=DIRECTION('ref_axis',(1.,0.,0.));
#6058=DIRECTION('center_axis',(0.,0.,1.));
#6059=DIRECTION('ref_axis',(1.,0.,0.));
#6060=DIRECTION('',(0.,0.,-1.));
#6061=DIRECTION('center_axis',(0.,0.,1.));
#6062=DIRECTION('ref_axis',(1.,0.,0.));
#6063=DIRECTION('center_axis',(0.,0.,1.));
#6064=DIRECTION('ref_axis',(1.,0.,0.));
#6065=DIRECTION('center_axis',(0.,0.,1.));
#6066=DIRECTION('ref_axis',(1.,0.,0.));
#6067=DIRECTION('',(0.,0.,-1.));
#6068=DIRECTION('center_axis',(0.,0.,1.));
#6069=DIRECTION('ref_axis',(1.,0.,0.));
#6070=DIRECTION('axis',(0.,0.,1.));
#6071=DIRECTION('refdir',(1.,0.,0.));
#6072=DIRECTION('center_axis',(0.,0.,1.));
#6073=DIRECTION('ref_axis',(1.,0.,0.));
#6074=DIRECTION('',(0.,0.,-1.));
#6075=DIRECTION('center_axis',(0.,0.,-1.));
#6076=DIRECTION('ref_axis',(1.,0.,0.));
#6077=DIRECTION('center_axis',(0.,0.,1.));
#6078=DIRECTION('ref_axis',(1.,0.,0.));
#6079=DIRECTION('',(0.,0.,-1.));
#6080=DIRECTION('center_axis',(0.,0.,1.));
#6081=DIRECTION('ref_axis',(1.,0.,0.));
#6082=DIRECTION('',(0.,0.,-1.));
#6083=DIRECTION('center_axis',(0.,0.,1.));
#6084=DIRECTION('ref_axis',(1.,0.,0.));
#6085=DIRECTION('',(0.,0.,-1.));
#6086=DIRECTION('center_axis',(0.,0.,1.));
#6087=DIRECTION('ref_axis',(1.,0.,0.));
#6088=DIRECTION('',(0.,0.,-1.));
#6089=DIRECTION('center_axis',(0.,0.,1.));
#6090=DIRECTION('ref_axis',(1.,0.,0.));
#6091=DIRECTION('',(0.,0.,-1.));
#6092=DIRECTION('center_axis',(0.,0.,1.));
#6093=DIRECTION('ref_axis',(1.,0.,0.));
#6094=DIRECTION('',(0.,0.,-1.));
#6095=DIRECTION('center_axis',(0.,0.,1.));
#6096=DIRECTION('ref_axis',(1.,0.,0.));
#6097=DIRECTION('',(0.,0.,-1.));
#6098=DIRECTION('center_axis',(0.,0.,1.));
#6099=DIRECTION('ref_axis',(1.,0.,0.));
#6100=DIRECTION('',(0.,0.,-1.));
#6101=DIRECTION('center_axis',(0.,0.,1.));
#6102=DIRECTION('ref_axis',(1.,0.,0.));
#6103=DIRECTION('',(0.,0.,-1.));
#6104=DIRECTION('center_axis',(0.,0.,1.));
#6105=DIRECTION('ref_axis',(1.,0.,0.));
#6106=DIRECTION('',(0.,0.,-1.));
#6107=DIRECTION('center_axis',(0.,0.,1.));
#6108=DIRECTION('ref_axis',(1.,0.,0.));
#6109=DIRECTION('',(0.,0.,-1.));
#6110=DIRECTION('center_axis',(0.,0.,1.));
#6111=DIRECTION('ref_axis',(1.,0.,0.));
#6112=DIRECTION('',(0.,0.,-1.));
#6113=DIRECTION('center_axis',(0.,0.,1.));
#6114=DIRECTION('ref_axis',(1.,0.,0.));
#6115=DIRECTION('',(0.,0.,-1.));
#6116=DIRECTION('center_axis',(0.,0.,1.));
#6117=DIRECTION('ref_axis',(1.,0.,0.));
#6118=DIRECTION('',(0.,0.,-1.));
#6119=DIRECTION('center_axis',(0.,0.,1.));
#6120=DIRECTION('ref_axis',(1.,0.,0.));
#6121=DIRECTION('',(0.,0.,-1.));
#6122=DIRECTION('center_axis',(0.,0.,1.));
#6123=DIRECTION('ref_axis',(1.,0.,0.));
#6124=DIRECTION('',(0.,0.,-1.));
#6125=DIRECTION('center_axis',(0.,0.,1.));
#6126=DIRECTION('ref_axis',(1.,0.,0.));
#6127=DIRECTION('',(0.,0.,-1.));
#6128=DIRECTION('center_axis',(0.,0.,1.));
#6129=DIRECTION('ref_axis',(1.,0.,0.));
#6130=DIRECTION('',(0.,0.,-1.));
#6131=DIRECTION('center_axis',(0.,0.,1.));
#6132=DIRECTION('ref_axis',(1.,0.,0.));
#6133=DIRECTION('',(0.,0.,-1.));
#6134=DIRECTION('center_axis',(0.,0.,1.));
#6135=DIRECTION('ref_axis',(1.,0.,0.));
#6136=DIRECTION('',(0.,0.,-1.));
#6137=DIRECTION('center_axis',(0.,0.,1.));
#6138=DIRECTION('ref_axis',(1.,0.,0.));
#6139=DIRECTION('',(0.,0.,-1.));
#6140=DIRECTION('center_axis',(0.,0.,1.));
#6141=DIRECTION('ref_axis',(1.,0.,0.));
#6142=DIRECTION('',(0.,0.,-1.));
#6143=DIRECTION('center_axis',(0.,0.,1.));
#6144=DIRECTION('ref_axis',(1.,0.,0.));
#6145=DIRECTION('',(0.,0.,-1.));
#6146=DIRECTION('center_axis',(0.,0.,1.));
#6147=DIRECTION('ref_axis',(1.,0.,0.));
#6148=DIRECTION('',(0.,0.,-1.));
#6149=DIRECTION('center_axis',(0.,0.,1.));
#6150=DIRECTION('ref_axis',(1.,0.,0.));
#6151=DIRECTION('',(0.,0.,-1.));
#6152=DIRECTION('center_axis',(0.,0.,1.));
#6153=DIRECTION('ref_axis',(1.,0.,0.));
#6154=DIRECTION('',(0.,0.,-1.));
#6155=DIRECTION('center_axis',(0.,0.,1.));
#6156=DIRECTION('ref_axis',(1.,0.,0.));
#6157=DIRECTION('',(0.,0.,-1.));
#6158=DIRECTION('center_axis',(0.,0.,1.));
#6159=DIRECTION('ref_axis',(1.,0.,0.));
#6160=DIRECTION('',(0.,0.,-1.));
#6161=DIRECTION('center_axis',(0.,0.,1.));
#6162=DIRECTION('ref_axis',(1.,0.,0.));
#6163=DIRECTION('',(0.,0.,-1.));
#6164=DIRECTION('center_axis',(0.,0.,1.));
#6165=DIRECTION('ref_axis',(1.,0.,0.));
#6166=DIRECTION('',(0.,0.,-1.));
#6167=DIRECTION('center_axis',(0.,0.,1.));
#6168=DIRECTION('ref_axis',(1.,0.,0.));
#6169=DIRECTION('',(0.,0.,-1.));
#6170=DIRECTION('center_axis',(0.,0.,1.));
#6171=DIRECTION('ref_axis',(1.,0.,0.));
#6172=DIRECTION('',(0.,0.,-1.));
#6173=DIRECTION('center_axis',(0.,0.,1.));
#6174=DIRECTION('ref_axis',(1.,0.,0.));
#6175=DIRECTION('',(0.,0.,-1.));
#6176=DIRECTION('center_axis',(0.,0.,1.));
#6177=DIRECTION('ref_axis',(1.,0.,0.));
#6178=DIRECTION('',(0.,0.,-1.));
#6179=DIRECTION('center_axis',(0.,0.,-1.));
#6180=DIRECTION('ref_axis',(1.,0.,0.));
#6181=DIRECTION('center_axis',(0.,0.,1.));
#6182=DIRECTION('ref_axis',(0.409441503265782,-0.912336371851663,0.));
#6183=DIRECTION('',(0.,0.,1.));
#6184=DIRECTION('center_axis',(0.,0.,1.));
#6185=DIRECTION('ref_axis',(1.,-2.80853466614331E-13,0.));
#6186=DIRECTION('center_axis',(0.,0.,1.));
#6187=DIRECTION('ref_axis',(1.,-2.80853466614331E-13,0.));
#6188=DIRECTION('',(0.,0.,1.));
#6189=DIRECTION('center_axis',(0.,0.,1.));
#6190=DIRECTION('ref_axis',(1.,-2.80853466614331E-13,0.));
#6191=DIRECTION('',(0.,0.,1.));
#6192=DIRECTION('center_axis',(0.,0.,1.));
#6193=DIRECTION('ref_axis',(1.,-2.80853466614331E-13,0.));
#6194=DIRECTION('',(0.,0.,1.));
#6195=DIRECTION('center_axis',(0.,0.,1.));
#6196=DIRECTION('ref_axis',(1.,-2.80853466614331E-13,0.));
#6197=DIRECTION('',(0.,0.,1.));
#6198=DIRECTION('center_axis',(0.,0.,1.));
#6199=DIRECTION('ref_axis',(1.,-2.80853466614331E-13,0.));
#6200=DIRECTION('',(0.,0.,1.));
#6201=DIRECTION('center_axis',(0.,0.,1.));
#6202=DIRECTION('ref_axis',(1.,-2.80853466614331E-13,0.));
#6203=DIRECTION('',(0.,0.,1.));
#6204=DIRECTION('center_axis',(0.,0.,1.));
#6205=DIRECTION('ref_axis',(1.,-2.80853466614331E-13,0.));
#6206=DIRECTION('',(0.,0.,1.));
#6207=DIRECTION('center_axis',(0.,0.,1.));
#6208=DIRECTION('ref_axis',(1.,-2.80853466614331E-13,0.));
#6209=DIRECTION('',(0.,0.,1.));
#6210=DIRECTION('center_axis',(0.,0.,1.));
#6211=DIRECTION('ref_axis',(1.,-2.80853466614331E-13,0.));
#6212=DIRECTION('',(0.,0.,1.));
#6213=DIRECTION('center_axis',(0.,0.,1.));
#6214=DIRECTION('ref_axis',(1.,-2.80853466614331E-13,0.));
#6215=DIRECTION('',(0.,0.,1.));
#6216=DIRECTION('center_axis',(0.,0.,1.));
#6217=DIRECTION('ref_axis',(1.,-2.80853466614331E-13,0.));
#6218=DIRECTION('',(0.,0.,1.));
#6219=DIRECTION('center_axis',(0.,0.,1.));
#6220=DIRECTION('ref_axis',(1.,-2.80853466614331E-13,0.));
#6221=DIRECTION('',(0.,0.,1.));
#6222=DIRECTION('center_axis',(0.,0.,1.));
#6223=DIRECTION('ref_axis',(1.,-2.80853466614331E-13,0.));
#6224=DIRECTION('',(0.,0.,1.));
#6225=DIRECTION('center_axis',(0.,0.,1.));
#6226=DIRECTION('ref_axis',(1.,-2.80853466614331E-13,0.));
#6227=DIRECTION('',(0.,0.,1.));
#6228=DIRECTION('center_axis',(0.,0.,1.));
#6229=DIRECTION('ref_axis',(1.,-2.80853466614331E-13,0.));
#6230=DIRECTION('',(0.,0.,1.));
#6231=DIRECTION('center_axis',(0.,0.,1.));
#6232=DIRECTION('ref_axis',(1.,-2.80853466614331E-13,0.));
#6233=DIRECTION('',(0.,0.,1.));
#6234=DIRECTION('center_axis',(0.,0.,1.));
#6235=DIRECTION('ref_axis',(1.,-2.80853466614331E-13,0.));
#6236=DIRECTION('',(0.,0.,1.));
#6237=DIRECTION('center_axis',(0.,0.,1.));
#6238=DIRECTION('ref_axis',(1.,-2.80853466614331E-13,0.));
#6239=DIRECTION('',(0.,0.,1.));
#6240=DIRECTION('center_axis',(0.,0.,1.));
#6241=DIRECTION('ref_axis',(1.,-2.80853466614331E-13,0.));
#6242=DIRECTION('',(0.,0.,1.));
#6243=DIRECTION('center_axis',(0.,0.,1.));
#6244=DIRECTION('ref_axis',(1.,-2.80853466614331E-13,0.));
#6245=DIRECTION('',(0.,0.,1.));
#6246=DIRECTION('center_axis',(0.,0.,1.));
#6247=DIRECTION('ref_axis',(1.,-2.80853466614331E-13,0.));
#6248=DIRECTION('',(0.,0.,1.));
#6249=DIRECTION('center_axis',(0.,0.,1.));
#6250=DIRECTION('ref_axis',(1.,-2.80853466614331E-13,0.));
#6251=DIRECTION('',(0.,0.,1.));
#6252=DIRECTION('center_axis',(0.,0.,1.));
#6253=DIRECTION('ref_axis',(1.,-2.80853466614331E-13,0.));
#6254=DIRECTION('',(0.,0.,1.));
#6255=DIRECTION('center_axis',(0.,0.,1.));
#6256=DIRECTION('ref_axis',(1.,-2.80853466614331E-13,0.));
#6257=DIRECTION('',(0.,0.,1.));
#6258=DIRECTION('center_axis',(0.,0.,1.));
#6259=DIRECTION('ref_axis',(1.,-2.80853466614331E-13,0.));
#6260=DIRECTION('',(0.,0.,1.));
#6261=DIRECTION('center_axis',(0.,0.,1.));
#6262=DIRECTION('ref_axis',(1.,-2.80853466614331E-13,0.));
#6263=DIRECTION('',(0.,0.,1.));
#6264=DIRECTION('center_axis',(0.,0.,1.));
#6265=DIRECTION('ref_axis',(1.,-2.80853466614331E-13,0.));
#6266=DIRECTION('',(0.,0.,1.));
#6267=DIRECTION('center_axis',(0.,0.,1.));
#6268=DIRECTION('ref_axis',(1.,-2.80853466614331E-13,0.));
#6269=DIRECTION('',(0.,0.,1.));
#6270=DIRECTION('center_axis',(0.,0.,1.));
#6271=DIRECTION('ref_axis',(1.,-2.80853466614331E-13,0.));
#6272=DIRECTION('',(0.,0.,1.));
#6273=DIRECTION('center_axis',(0.,0.,1.));
#6274=DIRECTION('ref_axis',(1.,-2.80853466614331E-13,0.));
#6275=DIRECTION('',(0.,0.,1.));
#6276=DIRECTION('center_axis',(0.,0.,1.));
#6277=DIRECTION('ref_axis',(1.,-2.80853466614331E-13,0.));
#6278=DIRECTION('',(0.,0.,1.));
#6279=DIRECTION('center_axis',(0.,0.,1.));
#6280=DIRECTION('ref_axis',(1.,-2.80853466614331E-13,0.));
#6281=DIRECTION('',(0.,0.,1.));
#6282=DIRECTION('center_axis',(0.,0.,1.));
#6283=DIRECTION('ref_axis',(1.,-2.80853466614331E-13,0.));
#6284=DIRECTION('',(0.,0.,1.));
#6285=DIRECTION('center_axis',(0.,0.,1.));
#6286=DIRECTION('ref_axis',(1.,-2.80853466614331E-13,0.));
#6287=DIRECTION('center_axis',(0.,0.,-1.));
#6288=DIRECTION('ref_axis',(1.,-2.80853466614331E-13,0.));
#6289=DIRECTION('center_axis',(0.,0.,1.));
#6290=DIRECTION('ref_axis',(-0.942680984145002,-0.333695313319517,0.));
#6291=DIRECTION('center_axis',(0.,0.,-1.));
#6292=DIRECTION('ref_axis',(1.,0.,0.));
#6293=DIRECTION('center_axis',(-1.60246890531964E-16,-1.,0.));
#6294=DIRECTION('ref_axis',(1.,-1.60246890531964E-16,0.));
#6295=DIRECTION('',(1.,-1.60246890531964E-16,0.));
#6296=DIRECTION('',(0.,0.,1.));
#6297=DIRECTION('',(1.,-1.60246890531964E-16,0.));
#6298=DIRECTION('',(0.,0.,1.));
#6299=DIRECTION('center_axis',(-0.866025403784439,-0.5,0.));
#6300=DIRECTION('ref_axis',(0.5,-0.866025403784439,0.));
#6301=DIRECTION('',(0.5,-0.866025403784439,0.));
#6302=DIRECTION('',(0.,0.,1.));
#6303=DIRECTION('',(0.5,-0.866025403784439,0.));
#6304=DIRECTION('center_axis',(-0.866025403784439,0.5,0.));
#6305=DIRECTION('ref_axis',(-0.5,-0.866025403784439,0.));
#6306=DIRECTION('',(-0.5,-0.866025403784439,0.));
#6307=DIRECTION('',(0.,0.,1.));
#6308=DIRECTION('',(-0.5,-0.866025403784439,0.));
#6309=DIRECTION('center_axis',(1.60246890531964E-16,1.,0.));
#6310=DIRECTION('ref_axis',(-1.,1.60246890531964E-16,0.));
#6311=DIRECTION('',(-1.,1.60246890531964E-16,0.));
#6312=DIRECTION('',(0.,0.,1.));
#6313=DIRECTION('',(-1.,1.60246890531964E-16,0.));
#6314=DIRECTION('center_axis',(0.866025403784439,0.5,0.));
#6315=DIRECTION('ref_axis',(-0.5,0.866025403784439,0.));
#6316=DIRECTION('',(-0.5,0.866025403784439,0.));
#6317=DIRECTION('',(0.,0.,1.));
#6318=DIRECTION('',(-0.5,0.866025403784439,0.));
#6319=DIRECTION('center_axis',(0.866025403784439,-0.5,0.));
#6320=DIRECTION('ref_axis',(0.5,0.866025403784439,0.));
#6321=DIRECTION('',(0.5,0.866025403784439,0.));
#6322=DIRECTION('',(0.5,0.866025403784439,0.));
#6323=DIRECTION('center_axis',(0.,0.,1.));
#6324=DIRECTION('ref_axis',(1.,0.,0.));
#6325=DIRECTION('center_axis',(0.,0.,1.));
#6326=DIRECTION('ref_axis',(1.,0.,0.));
#6327=DIRECTION('center_axis',(0.,0.,1.));
#6328=DIRECTION('ref_axis',(1.,0.,0.));
#6329=DIRECTION('center_axis',(0.,0.,1.));
#6330=DIRECTION('ref_axis',(1.,0.,0.));
#6331=DIRECTION('',(0.,0.,-1.));
#6332=DIRECTION('center_axis',(0.,0.,1.));
#6333=DIRECTION('ref_axis',(1.,0.,0.));
#6334=DIRECTION('center_axis',(0.,0.,1.));
#6335=DIRECTION('ref_axis',(1.,0.,0.));
#6336=DIRECTION('center_axis',(0.,0.,1.));
#6337=DIRECTION('ref_axis',(1.,0.,0.));
#6338=DIRECTION('axis',(0.,0.,1.));
#6339=DIRECTION('refdir',(1.,0.,0.));
#6340=DIRECTION('center_axis',(0.,0.,-1.));
#6341=DIRECTION('ref_axis',(-0.949090833458245,0.315002523554231,0.));
#6342=DIRECTION('',(0.,0.,-1.));
#6343=DIRECTION('center_axis',(0.,0.,-1.));
#6344=DIRECTION('ref_axis',(1.,0.,0.));
#6345=DIRECTION('center_axis',(0.,0.,-1.));
#6346=DIRECTION('ref_axis',(1.,0.,0.));
#6347=DIRECTION('',(0.,0.,-1.));
#6348=DIRECTION('center_axis',(0.,0.,-1.));
#6349=DIRECTION('ref_axis',(1.,0.,0.));
#6350=DIRECTION('center_axis',(0.,0.,-1.));
#6351=DIRECTION('ref_axis',(1.,0.,0.));
#6352=DIRECTION('',(0.,0.,-1.));
#6353=DIRECTION('center_axis',(0.,0.,-1.));
#6354=DIRECTION('ref_axis',(1.,0.,0.));
#6355=DIRECTION('',(0.,0.,-1.));
#6356=DIRECTION('center_axis',(0.,0.,-1.));
#6357=DIRECTION('ref_axis',(1.,0.,0.));
#6358=DIRECTION('',(0.,0.,-1.));
#6359=DIRECTION('center_axis',(0.,0.,-1.));
#6360=DIRECTION('ref_axis',(0.938432355146259,-0.345463044064985,0.));
#6361=DIRECTION('',(0.,0.,-1.));
#6362=DIRECTION('center_axis',(0.,0.,-1.));
#6363=DIRECTION('ref_axis',(1.,0.,0.));
#6364=DIRECTION('center_axis',(0.,0.,-1.));
#6365=DIRECTION('ref_axis',(0.0179423478205307,0.999839023120566,0.));
#6366=DIRECTION('',(1.22464679914735E-16,-6.20582083667111E-32,-1.));
#6367=DIRECTION('center_axis',(0.,0.,1.));
#6368=DIRECTION('ref_axis',(1.,-3.8427904741888E-16,0.));
#6369=DIRECTION('center_axis',(0.,0.,-1.));
#6370=DIRECTION('ref_axis',(1.,-3.8427904741888E-16,0.));
#6371=DIRECTION('',(1.22464679914735E-16,-6.20582083667111E-32,-1.));
#6372=DIRECTION('center_axis',(0.,0.,-1.));
#6373=DIRECTION('ref_axis',(1.,-3.8427904741888E-16,0.));
#6374=DIRECTION('',(1.22464679914735E-16,-6.20582083667111E-32,-1.));
#6375=DIRECTION('center_axis',(0.,0.,-1.));
#6376=DIRECTION('ref_axis',(1.,-3.8427904741888E-16,0.));
#6377=DIRECTION('',(1.22464679914735E-16,-6.20582083667111E-32,-1.));
#6378=DIRECTION('center_axis',(0.,0.,-1.));
#6379=DIRECTION('ref_axis',(1.,-3.8427904741888E-16,0.));
#6380=DIRECTION('',(1.22464679914735E-16,-6.20582083667111E-32,-1.));
#6381=DIRECTION('center_axis',(0.,0.,-1.));
#6382=DIRECTION('ref_axis',(-0.609355746674506,-0.79289695042594,0.));
#6383=DIRECTION('',(1.22464679914735E-16,-6.20582083667111E-32,-1.));
#6384=DIRECTION('center_axis',(0.,0.,-1.));
#6385=DIRECTION('ref_axis',(1.,-3.8427904741888E-16,0.));
#6386=DIRECTION('center_axis',(0.,0.,-1.));
#6387=DIRECTION('ref_axis',(1.,-3.8427904741888E-16,0.));
#6388=DIRECTION('center_axis',(0.,0.,1.));
#6389=DIRECTION('ref_axis',(1.,0.,0.));
#6390=DIRECTION('',(0.5,0.866025403784439,0.));
#6391=DIRECTION('',(-0.5,0.866025403784439,0.));
#6392=DIRECTION('',(-1.,1.37354477598826E-16,0.));
#6393=DIRECTION('',(-0.5,-0.866025403784439,0.));
#6394=DIRECTION('',(0.5,-0.866025403784439,0.));
#6395=DIRECTION('',(1.,-1.37354477598826E-16,0.));
#6396=DIRECTION('center_axis',(0.,0.,-1.));
#6397=DIRECTION('ref_axis',(1.,0.,0.));
#6398=DIRECTION('center_axis',(-1.37354477598826E-16,-1.,0.));
#6399=DIRECTION('ref_axis',(1.,-1.37354477598826E-16,0.));
#6400=DIRECTION('',(1.,-1.37354477598826E-16,0.));
#6401=DIRECTION('',(0.,0.,1.));
#6402=DIRECTION('',(0.,0.,1.));
#6403=DIRECTION('center_axis',(-0.866025403784439,-0.5,0.));
#6404=DIRECTION('ref_axis',(0.5,-0.866025403784439,0.));
#6405=DIRECTION('',(0.5,-0.866025403784439,0.));
#6406=DIRECTION('',(0.,0.,1.));
#6407=DIRECTION('center_axis',(-0.866025403784439,0.5,0.));
#6408=DIRECTION('ref_axis',(-0.5,-0.866025403784439,0.));
#6409=DIRECTION('',(-0.5,-0.866025403784439,0.));
#6410=DIRECTION('',(0.,0.,1.));
#6411=DIRECTION('center_axis',(1.37354477598826E-16,1.,0.));
#6412=DIRECTION('ref_axis',(-1.,1.37354477598826E-16,0.));
#6413=DIRECTION('',(-1.,1.37354477598826E-16,0.));
#6414=DIRECTION('',(0.,0.,1.));
#6415=DIRECTION('center_axis',(0.866025403784439,0.5,0.));
#6416=DIRECTION('ref_axis',(-0.5,0.866025403784439,0.));
#6417=DIRECTION('',(-0.5,0.866025403784439,0.));
#6418=DIRECTION('',(0.,0.,1.));
#6419=DIRECTION('center_axis',(0.866025403784439,-0.5,0.));
#6420=DIRECTION('ref_axis',(0.5,0.866025403784439,0.));
#6421=DIRECTION('',(0.5,0.866025403784439,0.));
#6422=DIRECTION('center_axis',(0.,0.,1.));
#6423=DIRECTION('ref_axis',(1.,0.,0.));
#6424=DIRECTION('axis',(0.,0.,1.));
#6425=DIRECTION('refdir',(1.,0.,0.));
#6426=DIRECTION('center_axis',(0.,0.,1.));
#6427=DIRECTION('ref_axis',(1.,0.,0.));
#6428=DIRECTION('center_axis',(0.,0.,1.));
#6429=DIRECTION('ref_axis',(1.,0.,0.));
#6430=DIRECTION('',(0.,0.,-1.));
#6431=DIRECTION('center_axis',(0.,0.,1.));
#6432=DIRECTION('ref_axis',(1.,0.,0.));
#6433=DIRECTION('center_axis',(0.,0.,1.));
#6434=DIRECTION('ref_axis',(1.,0.,0.));
#6435=DIRECTION('center_axis',(0.,0.,1.));
#6436=DIRECTION('ref_axis',(1.,0.,0.));
#6437=DIRECTION('',(0.,0.,1.));
#6438=DIRECTION('',(1.,0.,0.));
#6439=DIRECTION('',(1.22464679914735E-16,0.,-1.));
#6440=DIRECTION('',(-1.,0.,-1.22464679914735E-16));
#6441=DIRECTION('',(0.,0.,1.));
#6442=DIRECTION('',(1.,0.,0.));
#6443=DIRECTION('',(0.,0.,1.));
#6444=DIRECTION('',(1.,0.,0.));
#6445=DIRECTION('',(0.,0.,1.));
#6446=DIRECTION('',(1.,0.,0.));
#6447=DIRECTION('',(0.,0.,1.));
#6448=DIRECTION('',(1.,0.,0.));
#6449=DIRECTION('',(0.,0.,1.));
#6450=DIRECTION('',(1.,0.,0.));
#6451=DIRECTION('',(0.,0.,1.));
#6452=DIRECTION('',(1.,0.,0.));
#6453=DIRECTION('',(0.,0.,1.));
#6454=DIRECTION('',(1.,0.,0.));
#6455=DIRECTION('',(-1.,0.,0.));
#6456=DIRECTION('',(0.,-0.5,0.866025403784439));
#6457=DIRECTION('',(-1.,0.,0.));
#6458=DIRECTION('',(0.,-1.,0.));
#6459=DIRECTION('',(1.,0.,2.22044604925031E-16));
#6460=DIRECTION('',(2.22044604925031E-16,0.,-1.));
#6461=DIRECTION('',(1.22464679914735E-16,0.,-1.));
#6462=DIRECTION('',(-1.,0.,-1.22464679914735E-16));
#6463=DIRECTION('',(0.,-1.,0.));
#6464=DIRECTION('',(0.5,5.55111512312578E-17,0.866025403784439));
#6465=DIRECTION('',(0.,-1.,0.));
#6466=DIRECTION('',(1.,0.,0.));
#6467=DIRECTION('',(-1.,0.,0.));
#6468=DIRECTION('',(0.,-0.5,0.866025403784439));
#6469=DIRECTION('',(-1.,0.,0.));
#6470=DIRECTION('',(0.,-1.,0.));
#6471=DIRECTION('',(0.,-1.,0.));
#6472=DIRECTION('',(0.5,5.55111512312578E-17,0.866025403784439));
#6473=DIRECTION('',(0.,-1.,0.));
#6474=DIRECTION('',(1.,0.,0.));
#6475=DIRECTION('',(0.,0.,1.));
#6476=DIRECTION('',(1.,0.,0.));
#6477=DIRECTION('',(1.22464679914735E-16,0.,-1.));
#6478=DIRECTION('',(-1.,0.,-1.22464679914735E-16));
#6479=DIRECTION('',(0.,0.,1.));
#6480=DIRECTION('',(1.,0.,0.));
#6481=DIRECTION('',(1.22464679914735E-16,0.,-1.));
#6482=DIRECTION('',(-1.,0.,-1.22464679914735E-16));
#6483=DIRECTION('',(0.,0.,1.));
#6484=DIRECTION('',(1.,0.,0.));
#6485=DIRECTION('',(0.,0.,1.));
#6486=DIRECTION('',(1.,0.,0.));
#6487=DIRECTION('',(0.,0.,1.));
#6488=DIRECTION('',(1.,0.,0.));
#6489=DIRECTION('',(0.,0.,1.));
#6490=DIRECTION('',(1.,0.,0.));
#6491=DIRECTION('',(0.,0.,1.));
#6492=DIRECTION('',(1.,0.,0.));
#6493=DIRECTION('',(0.,0.,1.));
#6494=DIRECTION('',(1.,0.,0.));
#6495=DIRECTION('',(-1.,0.,0.));
#6496=DIRECTION('',(0.,-0.5,0.866025403784439));
#6497=DIRECTION('',(-1.,0.,0.));
#6498=DIRECTION('',(0.,-1.,0.));
#6499=DIRECTION('',(0.,-1.,0.));
#6500=DIRECTION('',(0.5,5.55111512312578E-17,0.866025403784439));
#6501=DIRECTION('',(0.,-1.,0.));
#6502=DIRECTION('',(1.,0.,0.));
#6503=DIRECTION('',(-1.,0.,0.));
#6504=DIRECTION('',(0.,-0.5,0.866025403784439));
#6505=DIRECTION('',(-1.,0.,0.));
#6506=DIRECTION('',(0.,-1.,0.));
#6507=DIRECTION('',(0.,-1.,0.));
#6508=DIRECTION('',(0.5,5.55111512312578E-17,0.866025403784439));
#6509=DIRECTION('',(0.,-1.,0.));
#6510=DIRECTION('',(1.,0.,0.));
#6511=DIRECTION('',(1.,0.,2.22044604925031E-16));
#6512=DIRECTION('',(2.22044604925031E-16,0.,-1.));
#6513=DIRECTION('',(1.,0.,2.22044604925031E-16));
#6514=DIRECTION('',(2.22044604925031E-16,0.,-1.));
#6515=DIRECTION('',(1.,0.,2.22044604925031E-16));
#6516=DIRECTION('',(2.22044604925031E-16,0.,-1.));
#6517=CARTESIAN_POINT('',(0.,0.,0.));
#6518=CARTESIAN_POINT('',(0.,0.,0.));
#6519=CARTESIAN_POINT('Origin',(0.,1.6,60.));
#6520=CARTESIAN_POINT('',(0.,1.6,60.5));
#6521=CARTESIAN_POINT('Origin',(0.,1.6,60.));
#6522=CARTESIAN_POINT('',(0.45,1.6,60.5));
#6523=CARTESIAN_POINT('',(0.,1.6,60.5));
#6524=CARTESIAN_POINT('Origin',(0.45,1.6,60.));
#6525=CARTESIAN_POINT('Origin',(0.45,1.6,60.));
#6526=CARTESIAN_POINT('',(0.45,1.6,60.225));
#6527=CARTESIAN_POINT('Origin',(0.45,1.6,60.));
#6528=CARTESIAN_POINT('Origin',(0.,1.6,120.));
#6529=CARTESIAN_POINT('',(0.,1.6,120.5));
#6530=CARTESIAN_POINT('Origin',(0.,1.6,120.));
#6531=CARTESIAN_POINT('',(0.45,1.6,120.5));
#6532=CARTESIAN_POINT('',(0.,1.6,120.5));
#6533=CARTESIAN_POINT('Origin',(0.45,1.6,120.));
#6534=CARTESIAN_POINT('Origin',(0.45,1.6,120.));
#6535=CARTESIAN_POINT('',(0.45,1.6,120.225));
#6536=CARTESIAN_POINT('Origin',(0.45,1.6,120.));
#6537=CARTESIAN_POINT('Origin',(0.,51.,60.));
#6538=CARTESIAN_POINT('',(0.,51.,60.41));
#6539=CARTESIAN_POINT('Origin',(0.,51.,60.));
#6540=CARTESIAN_POINT('',(1.5,51.,60.41));
#6541=CARTESIAN_POINT('',(0.,51.,60.41));
#6542=CARTESIAN_POINT('Origin',(1.5,51.,60.));
#6543=CARTESIAN_POINT('Origin',(1.5,51.,60.));
#6544=CARTESIAN_POINT('Origin',(0.,9.,120.));
#6545=CARTESIAN_POINT('',(0.,9.,120.41));
#6546=CARTESIAN_POINT('Origin',(0.,9.,120.));
#6547=CARTESIAN_POINT('',(1.5,9.,120.41));
#6548=CARTESIAN_POINT('',(0.,9.,120.41));
#6549=CARTESIAN_POINT('Origin',(1.5,9.,120.));
#6550=CARTESIAN_POINT('Origin',(1.5,9.,120.));
#6551=CARTESIAN_POINT('Origin',(0.,9.,60.));
#6552=CARTESIAN_POINT('',(0.,9.,60.41));
#6553=CARTESIAN_POINT('Origin',(0.,9.,60.));
#6554=CARTESIAN_POINT('',(1.5,9.,60.41));
#6555=CARTESIAN_POINT('',(0.,9.,60.41));
#6556=CARTESIAN_POINT('Origin',(1.5,9.,60.));
#6557=CARTESIAN_POINT('Origin',(1.5,9.,60.));
#6558=CARTESIAN_POINT('Origin',(0.,51.,120.));
#6559=CARTESIAN_POINT('',(0.,51.,120.41));
#6560=CARTESIAN_POINT('Origin',(0.,51.,120.));
#6561=CARTESIAN_POINT('',(1.5,51.,120.41));
#6562=CARTESIAN_POINT('',(0.,51.,120.41));
#6563=CARTESIAN_POINT('Origin',(1.5,51.,120.));
#6564=CARTESIAN_POINT('Origin',(1.5,51.,120.));
#6565=CARTESIAN_POINT('Origin',(1.8,1.6,60.));
#6566=CARTESIAN_POINT('',(1.8,1.6,60.225));
#6567=CARTESIAN_POINT('Origin',(1.8,1.6,60.));
#6568=CARTESIAN_POINT('',(1.8,1.6,60.225));
#6569=CARTESIAN_POINT('Origin',(1.8,1.6,120.));
#6570=CARTESIAN_POINT('',(1.8,1.6,120.225));
#6571=CARTESIAN_POINT('Origin',(1.8,1.6,120.));
#6572=CARTESIAN_POINT('',(1.8,1.6,120.225));
#6573=CARTESIAN_POINT('Origin',(1.81,58.82,0.));
#6574=CARTESIAN_POINT('',(1.3,58.82,89.08));
#6575=CARTESIAN_POINT('',(1.8,58.82,89.08));
#6576=CARTESIAN_POINT('',(1.6825,58.82,89.08));
#6577=CARTESIAN_POINT('',(1.3,58.82,1.82));
#6578=CARTESIAN_POINT('',(1.3,58.82,0.));
#6579=CARTESIAN_POINT('',(1.8,58.82,1.82));
#6580=CARTESIAN_POINT('',(1.6825,58.82,1.82));
#6581=CARTESIAN_POINT('',(1.8,58.82,0.));
#6582=CARTESIAN_POINT('Origin',(1.81,58.82,0.));
#6583=CARTESIAN_POINT('',(1.3,58.82,178.18));
#6584=CARTESIAN_POINT('',(1.8,58.82,178.18));
#6585=CARTESIAN_POINT('',(1.6825,58.82,178.18));
#6586=CARTESIAN_POINT('',(1.3,58.82,90.92));
#6587=CARTESIAN_POINT('',(1.3,58.82,0.));
#6588=CARTESIAN_POINT('',(1.8,58.82,90.92));
#6589=CARTESIAN_POINT('',(1.6825,58.82,90.92));
#6590=CARTESIAN_POINT('',(1.8,58.82,0.));
#6591=CARTESIAN_POINT('Origin',(1.3,58.18,0.));
#6592=CARTESIAN_POINT('',(1.8,58.18,89.08));
#6593=CARTESIAN_POINT('',(1.3,58.18,89.08));
#6594=CARTESIAN_POINT('',(1.4275,58.18,89.08));
#6595=CARTESIAN_POINT('',(1.8,58.18,1.82));
#6596=CARTESIAN_POINT('',(1.8,58.18,0.));
#6597=CARTESIAN_POINT('',(1.3,58.18,1.82));
#6598=CARTESIAN_POINT('',(1.4275,58.18,1.82));
#6599=CARTESIAN_POINT('',(1.3,58.18,0.));
#6600=CARTESIAN_POINT('Origin',(1.3,58.18,0.));
#6601=CARTESIAN_POINT('',(1.8,58.18,178.18));
#6602=CARTESIAN_POINT('',(1.3,58.18,178.18));
#6603=CARTESIAN_POINT('',(1.4275,58.18,178.18));
#6604=CARTESIAN_POINT('',(1.8,58.18,90.92));
#6605=CARTESIAN_POINT('',(1.8,58.18,0.));
#6606=CARTESIAN_POINT('',(1.3,58.18,90.92));
#6607=CARTESIAN_POINT('',(1.4275,58.18,90.92));
#6608=CARTESIAN_POINT('',(1.3,58.18,0.));
#6609=CARTESIAN_POINT('Origin',(1.3,60.,178.18));
#6610=CARTESIAN_POINT('',(1.3,60.,178.18));
#6611=CARTESIAN_POINT('',(1.3,60.,178.18));
#6612=CARTESIAN_POINT('',(1.3,60.,180.));
#6613=CARTESIAN_POINT('',(1.3,60.,89.09));
#6614=CARTESIAN_POINT('',(1.3,0.,180.));
#6615=CARTESIAN_POINT('',(1.3,45.,180.));
#6616=CARTESIAN_POINT('',(1.3,0.,178.18));
#6617=CARTESIAN_POINT('',(1.3,0.,89.09));
#6618=CARTESIAN_POINT('',(1.3,60.,178.18));
#6619=CARTESIAN_POINT('',(1.3,0.,90.92));
#6620=CARTESIAN_POINT('',(1.3,60.,90.92));
#6621=CARTESIAN_POINT('',(1.3,0.,89.08));
#6622=CARTESIAN_POINT('',(1.3,0.,44.54));
#6623=CARTESIAN_POINT('',(1.3,60.,89.08));
#6624=CARTESIAN_POINT('',(1.3,0.,1.82));
#6625=CARTESIAN_POINT('',(1.3,60.,1.82));
#6626=CARTESIAN_POINT('',(1.3,0.,0.));
#6627=CARTESIAN_POINT('',(1.3,0.,0.));
#6628=CARTESIAN_POINT('',(1.3,60.,0.));
#6629=CARTESIAN_POINT('',(1.3,45.,0.));
#6630=CARTESIAN_POINT('',(1.3,60.,1.82));
#6631=CARTESIAN_POINT('',(1.3,60.,0.));
#6632=CARTESIAN_POINT('',(1.3,60.,1.82));
#6633=CARTESIAN_POINT('',(1.3,60.,89.08));
#6634=CARTESIAN_POINT('',(1.3,60.,89.08));
#6635=CARTESIAN_POINT('',(1.3,60.,90.92));
#6636=CARTESIAN_POINT('',(1.3,60.,44.54));
#6637=CARTESIAN_POINT('',(1.3,60.,90.92));
#6638=CARTESIAN_POINT('Origin',(1.555,30.,178.18));
#6639=CARTESIAN_POINT('',(1.8,0.,178.18));
#6640=CARTESIAN_POINT('',(0.7775,0.,178.18));
#6641=CARTESIAN_POINT('',(1.8,15.,178.18));
#6642=CARTESIAN_POINT('Origin',(1.555,30.,178.18));
#6643=CARTESIAN_POINT('',(1.8,60.,178.18));
#6644=CARTESIAN_POINT('',(1.8,15.,178.18));
#6645=CARTESIAN_POINT('',(1.6775,60.,178.18));
#6646=CARTESIAN_POINT('Origin',(1.8,0.,0.));
#6647=CARTESIAN_POINT('',(1.8,0.,90.92));
#6648=CARTESIAN_POINT('',(1.8,0.,0.));
#6649=CARTESIAN_POINT('',(1.8,15.,90.92));
#6650=CARTESIAN_POINT('Origin',(1.8,0.,0.));
#6651=CARTESIAN_POINT('',(1.8,60.,90.92));
#6652=CARTESIAN_POINT('',(1.8,15.,90.92));
#6653=CARTESIAN_POINT('',(1.8,60.,0.));
#6654=CARTESIAN_POINT('Origin',(1.555,30.,90.92));
#6655=CARTESIAN_POINT('',(0.7775,0.,90.92));
#6656=CARTESIAN_POINT('Origin',(1.555,30.,90.92));
#6657=CARTESIAN_POINT('',(1.6775,60.,90.92));
#6658=CARTESIAN_POINT('Origin',(1.555,30.,89.08));
#6659=CARTESIAN_POINT('',(1.8,0.,89.08));
#6660=CARTESIAN_POINT('',(0.7775,0.,89.08));
#6661=CARTESIAN_POINT('',(1.8,15.,89.08));
#6662=CARTESIAN_POINT('Origin',(1.555,30.,89.08));
#6663=CARTESIAN_POINT('',(1.8,60.,89.08));
#6664=CARTESIAN_POINT('',(1.8,15.,89.08));
#6665=CARTESIAN_POINT('',(1.6775,60.,89.08));
#6666=CARTESIAN_POINT('Origin',(1.8,0.,0.));
#6667=CARTESIAN_POINT('',(1.8,0.,1.82));
#6668=CARTESIAN_POINT('',(1.8,0.,0.));
#6669=CARTESIAN_POINT('',(1.8,15.,1.82));
#6670=CARTESIAN_POINT('Origin',(1.8,0.,0.));
#6671=CARTESIAN_POINT('',(1.8,60.,1.82));
#6672=CARTESIAN_POINT('',(1.8,15.,1.82));
#6673=CARTESIAN_POINT('',(1.8,60.,0.));
#6674=CARTESIAN_POINT('Origin',(1.555,30.,1.82));
#6675=CARTESIAN_POINT('',(0.7775,0.,1.82));
#6676=CARTESIAN_POINT('Origin',(1.555,30.,1.82));
#6677=CARTESIAN_POINT('',(1.6775,60.,1.82));
#6678=CARTESIAN_POINT('Origin',(1.8,60.,0.));
#6679=CARTESIAN_POINT('',(0.,60.,0.));
#6680=CARTESIAN_POINT('',(1.8,60.,0.));
#6681=CARTESIAN_POINT('',(0.,60.,180.));
#6682=CARTESIAN_POINT('',(0.,60.,0.));
#6683=CARTESIAN_POINT('',(1.8,60.,180.));
#6684=CARTESIAN_POINT('Origin',(0.9,30.,0.));
#6685=CARTESIAN_POINT('',(0.,0.,0.));
#6686=CARTESIAN_POINT('',(0.,0.,0.));
#6687=CARTESIAN_POINT('',(0.,60.,0.));
#6688=CARTESIAN_POINT('Origin',(0.,0.,0.));
#6689=CARTESIAN_POINT('',(0.,0.,180.));
#6690=CARTESIAN_POINT('',(0.,0.,180.));
#6691=CARTESIAN_POINT('',(0.,0.,0.));
#6692=CARTESIAN_POINT('Origin',(0.,60.,0.));
#6693=CARTESIAN_POINT('',(0.,60.,180.));
#6694=CARTESIAN_POINT('Origin',(0.9,30.,180.));
#6695=CARTESIAN_POINT('',(0.,0.,0.));
#6696=CARTESIAN_POINT('Origin',(0.,51.,60.));
#6697=CARTESIAN_POINT('',(0.,51.,60.41));
#6698=CARTESIAN_POINT('Origin',(0.,51.,60.));
#6699=CARTESIAN_POINT('',(1.5,51.,60.41));
#6700=CARTESIAN_POINT('',(0.,51.,60.41));
#6701=CARTESIAN_POINT('Origin',(1.5,51.,60.));
#6702=CARTESIAN_POINT('Origin',(1.5,51.,60.));
#6703=CARTESIAN_POINT('Origin',(0.,9.,120.));
#6704=CARTESIAN_POINT('',(0.,9.,120.41));
#6705=CARTESIAN_POINT('Origin',(0.,9.,120.));
#6706=CARTESIAN_POINT('',(1.5,9.,120.41));
#6707=CARTESIAN_POINT('',(0.,9.,120.41));
#6708=CARTESIAN_POINT('Origin',(1.5,9.,120.));
#6709=CARTESIAN_POINT('Origin',(1.5,9.,120.));
#6710=CARTESIAN_POINT('Origin',(0.,9.,60.));
#6711=CARTESIAN_POINT('',(0.,9.,60.41));
#6712=CARTESIAN_POINT('Origin',(0.,9.,60.));
#6713=CARTESIAN_POINT('',(1.5,9.,60.41));
#6714=CARTESIAN_POINT('',(0.,9.,60.41));
#6715=CARTESIAN_POINT('Origin',(1.5,9.,60.));
#6716=CARTESIAN_POINT('Origin',(1.5,9.,60.));
#6717=CARTESIAN_POINT('Origin',(0.,51.,120.));
#6718=CARTESIAN_POINT('',(0.,51.,120.41));
#6719=CARTESIAN_POINT('Origin',(0.,51.,120.));
#6720=CARTESIAN_POINT('',(1.5,51.,120.41));
#6721=CARTESIAN_POINT('',(0.,51.,120.41));
#6722=CARTESIAN_POINT('Origin',(1.5,51.,120.));
#6723=CARTESIAN_POINT('Origin',(1.5,51.,120.));
#6724=CARTESIAN_POINT('Origin',(1.8,1.6,60.));
#6725=CARTESIAN_POINT('',(1.8,1.6,60.225));
#6726=CARTESIAN_POINT('Origin',(1.8,1.6,60.));
#6727=CARTESIAN_POINT('',(0.,1.6,60.225));
#6728=CARTESIAN_POINT('',(1.8,1.6,60.225));
#6729=CARTESIAN_POINT('Origin',(0.,1.6,60.));
#6730=CARTESIAN_POINT('Origin',(1.8,1.6,120.));
#6731=CARTESIAN_POINT('',(1.8,1.6,120.225));
#6732=CARTESIAN_POINT('Origin',(1.8,1.6,120.));
#6733=CARTESIAN_POINT('',(0.,1.6,120.225));
#6734=CARTESIAN_POINT('',(1.8,1.6,120.225));
#6735=CARTESIAN_POINT('Origin',(0.,1.6,120.));
#6736=CARTESIAN_POINT('Origin',(1.81,58.82,0.));
#6737=CARTESIAN_POINT('',(1.3,58.82,89.08));
#6738=CARTESIAN_POINT('',(1.8,58.82,89.08));
#6739=CARTESIAN_POINT('',(1.6825,58.82,89.08));
#6740=CARTESIAN_POINT('',(1.3,58.82,1.82));
#6741=CARTESIAN_POINT('',(1.3,58.82,0.));
#6742=CARTESIAN_POINT('',(1.8,58.82,1.82));
#6743=CARTESIAN_POINT('',(1.6825,58.82,1.82));
#6744=CARTESIAN_POINT('',(1.8,58.82,0.));
#6745=CARTESIAN_POINT('Origin',(1.81,58.82,0.));
#6746=CARTESIAN_POINT('',(1.3,58.82,178.18));
#6747=CARTESIAN_POINT('',(1.8,58.82,178.18));
#6748=CARTESIAN_POINT('',(1.6825,58.82,178.18));
#6749=CARTESIAN_POINT('',(1.3,58.82,90.92));
#6750=CARTESIAN_POINT('',(1.3,58.82,0.));
#6751=CARTESIAN_POINT('',(1.8,58.82,90.92));
#6752=CARTESIAN_POINT('',(1.6825,58.82,90.92));
#6753=CARTESIAN_POINT('',(1.8,58.82,0.));
#6754=CARTESIAN_POINT('Origin',(1.3,58.18,0.));
#6755=CARTESIAN_POINT('',(1.8,58.18,89.08));
#6756=CARTESIAN_POINT('',(1.3,58.18,89.08));
#6757=CARTESIAN_POINT('',(1.4275,58.18,89.08));
#6758=CARTESIAN_POINT('',(1.8,58.18,1.82));
#6759=CARTESIAN_POINT('',(1.8,58.18,0.));
#6760=CARTESIAN_POINT('',(1.3,58.18,1.82));
#6761=CARTESIAN_POINT('',(1.4275,58.18,1.82));
#6762=CARTESIAN_POINT('',(1.3,58.18,0.));
#6763=CARTESIAN_POINT('Origin',(1.3,58.18,0.));
#6764=CARTESIAN_POINT('',(1.8,58.18,178.18));
#6765=CARTESIAN_POINT('',(1.3,58.18,178.18));
#6766=CARTESIAN_POINT('',(1.4275,58.18,178.18));
#6767=CARTESIAN_POINT('',(1.8,58.18,90.92));
#6768=CARTESIAN_POINT('',(1.8,58.18,0.));
#6769=CARTESIAN_POINT('',(1.3,58.18,90.92));
#6770=CARTESIAN_POINT('',(1.4275,58.18,90.92));
#6771=CARTESIAN_POINT('',(1.3,58.18,0.));
#6772=CARTESIAN_POINT('Origin',(1.3,60.,178.18));
#6773=CARTESIAN_POINT('',(1.3,60.,178.18));
#6774=CARTESIAN_POINT('',(1.3,60.,178.18));
#6775=CARTESIAN_POINT('',(1.3,60.,180.));
#6776=CARTESIAN_POINT('',(1.3,60.,89.09));
#6777=CARTESIAN_POINT('',(1.3,0.,180.));
#6778=CARTESIAN_POINT('',(1.3,45.,180.));
#6779=CARTESIAN_POINT('',(1.3,0.,178.18));
#6780=CARTESIAN_POINT('',(1.3,0.,89.09));
#6781=CARTESIAN_POINT('',(1.3,60.,178.18));
#6782=CARTESIAN_POINT('',(1.3,0.,90.92));
#6783=CARTESIAN_POINT('',(1.3,60.,90.92));
#6784=CARTESIAN_POINT('',(1.3,0.,89.08));
#6785=CARTESIAN_POINT('',(1.3,0.,44.54));
#6786=CARTESIAN_POINT('',(1.3,60.,89.08));
#6787=CARTESIAN_POINT('',(1.3,0.,1.82));
#6788=CARTESIAN_POINT('',(1.3,60.,1.82));
#6789=CARTESIAN_POINT('',(1.3,0.,0.));
#6790=CARTESIAN_POINT('',(1.3,0.,0.));
#6791=CARTESIAN_POINT('',(1.3,60.,0.));
#6792=CARTESIAN_POINT('',(1.3,45.,0.));
#6793=CARTESIAN_POINT('',(1.3,60.,1.82));
#6794=CARTESIAN_POINT('',(1.3,60.,0.));
#6795=CARTESIAN_POINT('',(1.3,60.,1.82));
#6796=CARTESIAN_POINT('',(1.3,60.,89.08));
#6797=CARTESIAN_POINT('',(1.3,60.,89.08));
#6798=CARTESIAN_POINT('',(1.3,60.,90.92));
#6799=CARTESIAN_POINT('',(1.3,60.,44.54));
#6800=CARTESIAN_POINT('',(1.3,60.,90.92));
#6801=CARTESIAN_POINT('Origin',(1.555,30.,178.18));
#6802=CARTESIAN_POINT('',(1.8,0.,178.18));
#6803=CARTESIAN_POINT('',(0.7775,0.,178.18));
#6804=CARTESIAN_POINT('',(1.8,15.,178.18));
#6805=CARTESIAN_POINT('Origin',(1.555,30.,178.18));
#6806=CARTESIAN_POINT('',(1.8,60.,178.18));
#6807=CARTESIAN_POINT('',(1.8,15.,178.18));
#6808=CARTESIAN_POINT('',(1.6775,60.,178.18));
#6809=CARTESIAN_POINT('Origin',(1.8,0.,0.));
#6810=CARTESIAN_POINT('',(1.8,0.,90.92));
#6811=CARTESIAN_POINT('',(1.8,0.,0.));
#6812=CARTESIAN_POINT('',(1.8,15.,90.92));
#6813=CARTESIAN_POINT('Origin',(1.8,0.,0.));
#6814=CARTESIAN_POINT('',(1.8,60.,90.92));
#6815=CARTESIAN_POINT('',(1.8,15.,90.92));
#6816=CARTESIAN_POINT('',(1.8,60.,0.));
#6817=CARTESIAN_POINT('Origin',(1.555,30.,90.92));
#6818=CARTESIAN_POINT('',(0.7775,0.,90.92));
#6819=CARTESIAN_POINT('Origin',(1.555,30.,90.92));
#6820=CARTESIAN_POINT('',(1.6775,60.,90.92));
#6821=CARTESIAN_POINT('Origin',(1.555,30.,89.08));
#6822=CARTESIAN_POINT('',(1.8,0.,89.08));
#6823=CARTESIAN_POINT('',(0.7775,0.,89.08));
#6824=CARTESIAN_POINT('',(1.8,15.,89.08));
#6825=CARTESIAN_POINT('Origin',(1.555,30.,89.08));
#6826=CARTESIAN_POINT('',(1.8,60.,89.08));
#6827=CARTESIAN_POINT('',(1.8,15.,89.08));
#6828=CARTESIAN_POINT('',(1.6775,60.,89.08));
#6829=CARTESIAN_POINT('Origin',(1.8,0.,0.));
#6830=CARTESIAN_POINT('',(1.8,0.,1.82));
#6831=CARTESIAN_POINT('',(1.8,0.,0.));
#6832=CARTESIAN_POINT('',(1.8,15.,1.82));
#6833=CARTESIAN_POINT('Origin',(1.8,0.,0.));
#6834=CARTESIAN_POINT('',(1.8,60.,1.82));
#6835=CARTESIAN_POINT('',(1.8,15.,1.82));
#6836=CARTESIAN_POINT('',(1.8,60.,0.));
#6837=CARTESIAN_POINT('Origin',(1.555,30.,1.82));
#6838=CARTESIAN_POINT('',(0.7775,0.,1.82));
#6839=CARTESIAN_POINT('Origin',(1.555,30.,1.82));
#6840=CARTESIAN_POINT('',(1.6775,60.,1.82));
#6841=CARTESIAN_POINT('Origin',(1.8,60.,0.));
#6842=CARTESIAN_POINT('',(0.,60.,0.));
#6843=CARTESIAN_POINT('',(1.8,60.,0.));
#6844=CARTESIAN_POINT('',(0.,60.,180.));
#6845=CARTESIAN_POINT('',(0.,60.,0.));
#6846=CARTESIAN_POINT('',(1.8,60.,180.));
#6847=CARTESIAN_POINT('Origin',(0.9,30.,0.));
#6848=CARTESIAN_POINT('',(0.,0.,0.));
#6849=CARTESIAN_POINT('',(0.,0.,0.));
#6850=CARTESIAN_POINT('',(0.,60.,0.));
#6851=CARTESIAN_POINT('Origin',(0.,0.,0.));
#6852=CARTESIAN_POINT('',(0.,0.,180.));
#6853=CARTESIAN_POINT('',(0.,0.,180.));
#6854=CARTESIAN_POINT('',(0.,0.,0.));
#6855=CARTESIAN_POINT('Origin',(0.,60.,0.));
#6856=CARTESIAN_POINT('',(0.,60.,180.));
#6857=CARTESIAN_POINT('Origin',(0.9,30.,180.));
#6858=CARTESIAN_POINT('',(0.,0.,0.));
#6859=CARTESIAN_POINT('Origin',(0.,58.18,1.3));
#6860=CARTESIAN_POINT('',(57.36,58.18,1.8));
#6861=CARTESIAN_POINT('',(0.,58.18,1.8));
#6862=CARTESIAN_POINT('',(14.34,58.18,1.8));
#6863=CARTESIAN_POINT('',(57.36,58.18,1.3));
#6864=CARTESIAN_POINT('',(57.36,58.18,0.65));
#6865=CARTESIAN_POINT('',(0.,58.18,1.3));
#6866=CARTESIAN_POINT('',(0.,58.18,1.3));
#6867=CARTESIAN_POINT('',(0.,58.18,0.65));
#6868=CARTESIAN_POINT('Origin',(57.36,58.82,1.3));
#6869=CARTESIAN_POINT('',(0.,58.82,1.8));
#6870=CARTESIAN_POINT('',(57.36,58.82,1.8));
#6871=CARTESIAN_POINT('',(43.02,58.82,1.8));
#6872=CARTESIAN_POINT('',(0.,58.82,1.3));
#6873=CARTESIAN_POINT('',(0.,58.82,0.65));
#6874=CARTESIAN_POINT('',(57.36,58.82,1.3));
#6875=CARTESIAN_POINT('',(57.36,58.82,1.3));
#6876=CARTESIAN_POINT('',(57.36,58.82,0.65));
#6877=CARTESIAN_POINT('Origin',(28.68,58.5,1.3));
#6878=CARTESIAN_POINT('',(0.,59.25,1.3));
#6879=CARTESIAN_POINT('',(57.36,29.25,1.3));
#6880=CARTESIAN_POINT('Origin',(57.36,0.,0.));
#6881=CARTESIAN_POINT('',(57.36,0.,1.8));
#6882=CARTESIAN_POINT('',(57.36,0.,1.8));
#6883=CARTESIAN_POINT('',(57.36,0.,0.));
#6884=CARTESIAN_POINT('',(57.36,0.,0.));
#6885=CARTESIAN_POINT('',(57.36,60.,0.));
#6886=CARTESIAN_POINT('',(57.36,0.,0.));
#6887=CARTESIAN_POINT('',(57.36,60.,1.8));
#6888=CARTESIAN_POINT('',(57.36,60.,0.));
#6889=CARTESIAN_POINT('',(57.36,0.,1.8));
#6890=CARTESIAN_POINT('Origin',(28.68,30.,1.8));
#6891=CARTESIAN_POINT('',(0.,0.,1.8));
#6892=CARTESIAN_POINT('',(0.,60.,1.8));
#6893=CARTESIAN_POINT('',(0.,0.,1.8));
#6894=CARTESIAN_POINT('Origin',(57.36,60.,0.));
#6895=CARTESIAN_POINT('',(0.,60.,0.));
#6896=CARTESIAN_POINT('',(57.36,60.,0.));
#6897=CARTESIAN_POINT('',(0.,60.,1.8));
#6898=CARTESIAN_POINT('',(0.,60.,0.));
#6899=CARTESIAN_POINT('',(57.36,60.,1.8));
#6900=CARTESIAN_POINT('Origin',(0.,0.,0.));
#6901=CARTESIAN_POINT('',(0.,0.,0.));
#6902=CARTESIAN_POINT('',(0.,0.,0.));
#6903=CARTESIAN_POINT('',(0.,0.,0.));
#6904=CARTESIAN_POINT('Origin',(0.,60.,0.));
#6905=CARTESIAN_POINT('',(0.,60.,1.8));
#6906=CARTESIAN_POINT('',(0.,60.,0.));
#6907=CARTESIAN_POINT('Origin',(28.68,30.,1.8));
#6908=CARTESIAN_POINT('Origin',(28.68,30.,0.));
#6909=CARTESIAN_POINT('',(0.,0.,0.));
#6910=CARTESIAN_POINT('Origin',(57.36,0.6,0.));
#6911=CARTESIAN_POINT('',(57.36,0.6,0.));
#6912=CARTESIAN_POINT('',(0.,0.6,0.));
#6913=CARTESIAN_POINT('',(57.36,0.6,0.));
#6914=CARTESIAN_POINT('',(0.,0.6,177.36));
#6915=CARTESIAN_POINT('',(0.,0.6,0.));
#6916=CARTESIAN_POINT('',(57.36,0.6,177.36));
#6917=CARTESIAN_POINT('',(57.36,0.6,177.36));
#6918=CARTESIAN_POINT('',(57.36,0.6,0.));
#6919=CARTESIAN_POINT('Origin',(57.36,0.,0.));
#6920=CARTESIAN_POINT('',(57.36,0.,0.));
#6921=CARTESIAN_POINT('',(57.36,0.,0.));
#6922=CARTESIAN_POINT('',(57.36,0.,177.36));
#6923=CARTESIAN_POINT('',(57.36,0.,177.36));
#6924=CARTESIAN_POINT('',(57.36,0.,0.));
#6925=CARTESIAN_POINT('Origin',(0.,0.,0.));
#6926=CARTESIAN_POINT('',(0.,0.,0.));
#6927=CARTESIAN_POINT('',(0.,0.,0.));
#6928=CARTESIAN_POINT('',(0.,0.,177.36));
#6929=CARTESIAN_POINT('',(0.,0.,177.36));
#6930=CARTESIAN_POINT('',(0.,0.,0.));
#6931=CARTESIAN_POINT('Origin',(0.,0.6,0.));
#6932=CARTESIAN_POINT('',(0.,0.6,0.));
#6933=CARTESIAN_POINT('',(0.,0.6,177.36));
#6934=CARTESIAN_POINT('Origin',(28.68,0.3,177.36));
#6935=CARTESIAN_POINT('Origin',(28.68,0.3,0.));
#6936=CARTESIAN_POINT('',(0.,0.,0.));
#6937=CARTESIAN_POINT('Origin',(0.88,3.,0.));
#6938=CARTESIAN_POINT('',(0.88,3.,0.));
#6939=CARTESIAN_POINT('',(0.,3.,0.));
#6940=CARTESIAN_POINT('',(14.78,3.,0.));
#6941=CARTESIAN_POINT('',(0.88,3.,1.8));
#6942=CARTESIAN_POINT('',(0.88,3.,0.));
#6943=CARTESIAN_POINT('',(0.,3.,1.8));
#6944=CARTESIAN_POINT('',(14.78,3.,1.8));
#6945=CARTESIAN_POINT('',(0.,3.,0.));
#6946=CARTESIAN_POINT('Origin',(0.88,0.6,0.));
#6947=CARTESIAN_POINT('',(0.88,0.6,0.));
#6948=CARTESIAN_POINT('',(0.879999999999999,14.85,0.));
#6949=CARTESIAN_POINT('',(0.88,0.6,1.8));
#6950=CARTESIAN_POINT('',(0.88,0.6,0.));
#6951=CARTESIAN_POINT('',(0.879999999999999,14.85,1.8));
#6952=CARTESIAN_POINT('Origin',(0.,57.6,0.));
#6953=CARTESIAN_POINT('',(0.,57.6,1.8));
#6954=CARTESIAN_POINT('',(0.,57.6,1.8));
#6955=CARTESIAN_POINT('',(0.,57.6,0.));
#6956=CARTESIAN_POINT('',(0.,57.6,0.));
#6957=CARTESIAN_POINT('',(0.,57.6,0.));
#6958=CARTESIAN_POINT('Origin',(0.,0.6,0.));
#6959=CARTESIAN_POINT('',(57.36,0.6,0.));
#6960=CARTESIAN_POINT('',(0.,0.6,0.));
#6961=CARTESIAN_POINT('',(57.36,0.600000000000001,1.8));
#6962=CARTESIAN_POINT('',(57.36,0.6,0.));
#6963=CARTESIAN_POINT('',(0.,0.6,1.8));
#6964=CARTESIAN_POINT('Origin',(57.36,57.6,0.));
#6965=CARTESIAN_POINT('',(57.36,57.6,0.));
#6966=CARTESIAN_POINT('',(57.36,57.6,0.));
#6967=CARTESIAN_POINT('',(57.36,57.6,1.8));
#6968=CARTESIAN_POINT('',(57.36,57.6,1.8));
#6969=CARTESIAN_POINT('',(57.36,57.6,0.));
#6970=CARTESIAN_POINT('Origin',(57.36,0.6,0.));
#6971=CARTESIAN_POINT('',(57.36,0.6,0.));
#6972=CARTESIAN_POINT('',(57.36,0.6,1.8));
#6973=CARTESIAN_POINT('Origin',(28.68,29.1,1.8));
#6974=CARTESIAN_POINT('Origin',(28.68,29.1,0.));
#6975=CARTESIAN_POINT('',(0.,0.,0.));
#6976=CARTESIAN_POINT('Origin',(49.,-0.2,89.));
#6977=CARTESIAN_POINT('',(49.,-0.2,89.));
#6978=CARTESIAN_POINT('',(55.,-0.2,89.));
#6979=CARTESIAN_POINT('',(53.5,-0.2,89.));
#6980=CARTESIAN_POINT('',(49.,-2.,89.));
#6981=CARTESIAN_POINT('',(49.,-0.2,89.));
#6982=CARTESIAN_POINT('',(55.,-2.,89.));
#6983=CARTESIAN_POINT('',(25.7,-2.,89.));
#6984=CARTESIAN_POINT('',(55.,-0.2,89.));
#6985=CARTESIAN_POINT('Origin',(49.,-0.2,90.));
#6986=CARTESIAN_POINT('',(49.,-0.2,91.));
#6987=CARTESIAN_POINT('Origin',(49.,-0.2,90.));
#6988=CARTESIAN_POINT('',(49.,-2.,91.));
#6989=CARTESIAN_POINT('',(49.,-0.2,91.));
#6990=CARTESIAN_POINT('Origin',(49.,-2.,90.));
#6991=CARTESIAN_POINT('Origin',(55.,-0.2,91.));
#6992=CARTESIAN_POINT('',(55.,-0.2,91.));
#6993=CARTESIAN_POINT('',(56.5,-0.2,91.));
#6994=CARTESIAN_POINT('',(55.,-2.,91.));
#6995=CARTESIAN_POINT('',(55.,-0.2,91.));
#6996=CARTESIAN_POINT('',(28.7,-2.,91.));
#6997=CARTESIAN_POINT('Origin',(55.,-0.2,90.));
#6998=CARTESIAN_POINT('Origin',(55.,-0.2,90.));
#6999=CARTESIAN_POINT('Origin',(55.,-2.,90.));
#7000=CARTESIAN_POINT('Origin',(3.4,-0.2,60.));
#7001=CARTESIAN_POINT('',(3.175,-0.2,60.));
#7002=CARTESIAN_POINT('Origin',(3.4,-0.2,60.));
#7003=CARTESIAN_POINT('',(3.175,-2.,60.));
#7004=CARTESIAN_POINT('',(3.175,-0.2,60.));
#7005=CARTESIAN_POINT('Origin',(3.4,-2.,60.));
#7006=CARTESIAN_POINT('Origin',(3.4,-0.2,120.));
#7007=CARTESIAN_POINT('',(3.175,-0.2,120.));
#7008=CARTESIAN_POINT('Origin',(3.4,-0.2,120.));
#7009=CARTESIAN_POINT('',(3.175,-2.,120.));
#7010=CARTESIAN_POINT('',(3.175,-0.2,120.));
#7011=CARTESIAN_POINT('Origin',(3.4,-2.,120.));
#7012=CARTESIAN_POINT('Origin',(58.,-0.2,0.2));
#7013=CARTESIAN_POINT('',(58.,-0.2,0.2));
#7014=CARTESIAN_POINT('',(2.4,-0.2,0.2));
#7015=CARTESIAN_POINT('',(58.,-0.2,0.2));
#7016=CARTESIAN_POINT('',(2.4,-0.2,179.8));
#7017=CARTESIAN_POINT('',(2.4,-0.2,0.2));
#7018=CARTESIAN_POINT('',(58.,-0.2,179.8));
#7019=CARTESIAN_POINT('',(58.,-0.2,179.8));
#7020=CARTESIAN_POINT('',(58.,-0.2,0.2));
#7021=CARTESIAN_POINT('Origin',(58.,-2.,0.2));
#7022=CARTESIAN_POINT('',(58.,-2.,0.2));
#7023=CARTESIAN_POINT('',(58.,-2.,0.2));
#7024=CARTESIAN_POINT('',(58.,-2.,179.8));
#7025=CARTESIAN_POINT('',(58.,-2.,179.8));
#7026=CARTESIAN_POINT('',(58.,-2.,0.2));
#7027=CARTESIAN_POINT('Origin',(2.4,-2.,0.2));
#7028=CARTESIAN_POINT('',(2.4,-2.,0.2));
#7029=CARTESIAN_POINT('',(2.4,-2.,0.2));
#7030=CARTESIAN_POINT('',(2.4,-2.,179.8));
#7031=CARTESIAN_POINT('',(2.4,-2.,179.8));
#7032=CARTESIAN_POINT('',(2.4,-2.,0.2));
#7033=CARTESIAN_POINT('Origin',(2.4,-0.2,0.2));
#7034=CARTESIAN_POINT('',(2.4,-0.2,0.2));
#7035=CARTESIAN_POINT('',(2.4,-0.2,179.8));
#7036=CARTESIAN_POINT('Origin',(30.2,-1.1,179.8));
#7037=CARTESIAN_POINT('Origin',(30.2,-1.1,0.2));
#7038=CARTESIAN_POINT('',(0.,0.,0.));
#7039=CARTESIAN_POINT('Origin',(0.,2.,55.));
#7040=CARTESIAN_POINT('',(0.,2.,55.225));
#7041=CARTESIAN_POINT('Origin',(0.,2.,55.));
#7042=CARTESIAN_POINT('',(0.2,2.,55.225));
#7043=CARTESIAN_POINT('',(0.,2.,55.225));
#7044=CARTESIAN_POINT('Origin',(0.2,2.,55.));
#7045=CARTESIAN_POINT('Origin',(0.,2.,115.));
#7046=CARTESIAN_POINT('',(0.,2.,115.225));
#7047=CARTESIAN_POINT('Origin',(0.,2.,115.));
#7048=CARTESIAN_POINT('',(0.2,2.,115.225));
#7049=CARTESIAN_POINT('',(0.,2.,115.225));
#7050=CARTESIAN_POINT('Origin',(0.2,2.,115.));
#7051=CARTESIAN_POINT('Origin',(0.,0.,113.343333333333));
#7052=CARTESIAN_POINT('',(0.,0.42,113.343333333333));
#7053=CARTESIAN_POINT('',(0.,0.2,113.343333333333));
#7054=CARTESIAN_POINT('',(0.,1.5,113.343333333333));
#7055=CARTESIAN_POINT('',(0.2,0.369323706252388,113.343333333333));
#7056=CARTESIAN_POINT('Origin',(0.,0.,113.343333333333));
#7057=CARTESIAN_POINT('',(0.2,0.2,113.343333333333));
#7058=CARTESIAN_POINT('',(0.2,0.1,113.343333333333));
#7059=CARTESIAN_POINT('',(0.,0.2,113.343333333333));
#7060=CARTESIAN_POINT('Origin',(0.,0.,56.6566666666667));
#7061=CARTESIAN_POINT('',(0.,0.42,56.6566666666667));
#7062=CARTESIAN_POINT('',(0.,0.42,56.6566666666667));
#7063=CARTESIAN_POINT('',(0.2,0.369323706252388,56.6566666666667));
#7064=CARTESIAN_POINT('Origin',(0.,0.,56.6566666666667));
#7065=CARTESIAN_POINT('',(0.2,0.369323706252388,56.6566666666667));
#7066=CARTESIAN_POINT('Origin',(0.,0.,56.6566666666667));
#7067=CARTESIAN_POINT('',(0.,0.2,56.6566666666667));
#7068=CARTESIAN_POINT('',(0.,1.5,56.6566666666667));
#7069=CARTESIAN_POINT('',(0.2,0.2,56.6566666666667));
#7070=CARTESIAN_POINT('',(0.,0.2,56.6566666666667));
#7071=CARTESIAN_POINT('',(0.2,0.1,56.6566666666667));
#7072=CARTESIAN_POINT('Origin',(0.2,0.2,0.));
#7073=CARTESIAN_POINT('',(0.2,0.2,56.6466666666667));
#7074=CARTESIAN_POINT('',(0.2,0.2,0.));
#7075=CARTESIAN_POINT('',(0.2,0.346410161513776,56.6466666666667));
#7076=CARTESIAN_POINT('',(0.2,0.1,56.6466666666667));
#7077=CARTESIAN_POINT('',(0.2,0.346410161513776,0.));
#7078=CARTESIAN_POINT('',(0.2,0.346410161513776,0.));
#7079=CARTESIAN_POINT('',(0.2,3.,0.));
#7080=CARTESIAN_POINT('',(0.2,0.2,0.));
#7081=CARTESIAN_POINT('',(0.2,3.,170.));
#7082=CARTESIAN_POINT('',(0.2,3.,0.));
#7083=CARTESIAN_POINT('',(0.2,0.346410161513776,170.));
#7084=CARTESIAN_POINT('',(0.2,0.2,170.));
#7085=CARTESIAN_POINT('',(0.2,0.346410161513776,113.353333333333));
#7086=CARTESIAN_POINT('',(0.2,0.346410161513776,113.353333333333));
#7087=CARTESIAN_POINT('',(0.2,0.2,113.353333333333));
#7088=CARTESIAN_POINT('',(0.2,0.1,113.353333333333));
#7089=CARTESIAN_POINT('',(0.2,0.2,0.));
#7090=CARTESIAN_POINT('Origin',(0.,0.2,0.));
#7091=CARTESIAN_POINT('',(0.,0.2,0.));
#7092=CARTESIAN_POINT('',(0.,0.2,0.));
#7093=CARTESIAN_POINT('',(0.0916515138991168,0.2,0.));
#7094=CARTESIAN_POINT('',(0.,0.2,0.));
#7095=CARTESIAN_POINT('',(0.0916515138991168,0.2,56.6466666666667));
#7096=CARTESIAN_POINT('',(0.0916515138991168,0.2,0.));
#7097=CARTESIAN_POINT('',(0.,0.2,56.6466666666667));
#7098=CARTESIAN_POINT('Origin',(0.,0.2,0.));
#7099=CARTESIAN_POINT('',(0.0916515138991168,0.2,113.353333333333));
#7100=CARTESIAN_POINT('',(0.,0.2,113.353333333333));
#7101=CARTESIAN_POINT('',(0.0916515138991168,0.2,170.));
#7102=CARTESIAN_POINT('',(0.0916515138991168,0.2,113.353333333333));
#7103=CARTESIAN_POINT('',(0.,0.2,170.));
#7104=CARTESIAN_POINT('',(0.,0.2,170.));
#7105=CARTESIAN_POINT('',(0.,0.2,0.));
#7106=CARTESIAN_POINT('Origin',(0.,0.,113.353333333333));
#7107=CARTESIAN_POINT('',(0.,0.4,113.353333333333));
#7108=CARTESIAN_POINT('Origin',(0.,0.,113.353333333333));
#7109=CARTESIAN_POINT('',(0.,0.22,113.353333333333));
#7110=CARTESIAN_POINT('',(0.,1.5,113.353333333333));
#7111=CARTESIAN_POINT('Origin',(0.,0.,113.353333333333));
#7112=CARTESIAN_POINT('Origin',(0.,0.,113.353333333333));
#7113=CARTESIAN_POINT('',(0.,0.4,170.));
#7114=CARTESIAN_POINT('Origin',(0.,0.,170.));
#7115=CARTESIAN_POINT('',(0.,0.4,113.353333333333));
#7116=CARTESIAN_POINT('Origin',(0.,0.,113.353333333333));
#7117=CARTESIAN_POINT('',(0.,0.22,170.));
#7118=CARTESIAN_POINT('',(0.,0.22,113.353333333333));
#7119=CARTESIAN_POINT('Origin',(0.,0.,170.));
#7120=CARTESIAN_POINT('Origin',(0.1,1.6,170.));
#7121=CARTESIAN_POINT('',(0.,3.,170.));
#7122=CARTESIAN_POINT('',(0.2,3.,170.));
#7123=CARTESIAN_POINT('',(0.,3.,170.));
#7124=CARTESIAN_POINT('',(0.,3.,170.));
#7125=CARTESIAN_POINT('Origin',(0.,3.,0.));
#7126=CARTESIAN_POINT('',(0.,3.,0.));
#7127=CARTESIAN_POINT('',(0.,3.,0.));
#7128=CARTESIAN_POINT('',(0.,0.4,0.));
#7129=CARTESIAN_POINT('',(0.,3.,0.));
#7130=CARTESIAN_POINT('',(0.,0.4,56.6466666666667));
#7131=CARTESIAN_POINT('',(0.,0.4,0.));
#7132=CARTESIAN_POINT('',(0.,0.22,56.6466666666667));
#7133=CARTESIAN_POINT('',(0.,1.5,56.6466666666667));
#7134=CARTESIAN_POINT('',(0.,0.22,0.));
#7135=CARTESIAN_POINT('',(0.,0.22,0.));
#7136=CARTESIAN_POINT('',(0.,3.,0.));
#7137=CARTESIAN_POINT('Origin',(0.,0.,0.));
#7138=CARTESIAN_POINT('Origin',(0.,0.,0.));
#7139=CARTESIAN_POINT('Origin',(0.,0.,56.6466666666667));
#7140=CARTESIAN_POINT('Origin',(0.,0.,0.));
#7141=CARTESIAN_POINT('Origin',(0.,0.,56.6466666666667));
#7142=CARTESIAN_POINT('Origin',(0.,0.,0.));
#7143=CARTESIAN_POINT('Origin',(0.,0.,56.6466666666667));
#7144=CARTESIAN_POINT('Origin',(0.2,3.,0.));
#7145=CARTESIAN_POINT('',(0.2,3.,0.));
#7146=CARTESIAN_POINT('Origin',(0.1,1.6,0.));
#7147=CARTESIAN_POINT('',(0.,0.,0.));
#7148=CARTESIAN_POINT('Origin',(1.6,0.4,55.));
#7149=CARTESIAN_POINT('',(1.375,0.4,55.));
#7150=CARTESIAN_POINT('Origin',(1.6,0.4,55.));
#7151=CARTESIAN_POINT('',(1.375,0.2,55.));
#7152=CARTESIAN_POINT('',(1.375,0.4,55.));
#7153=CARTESIAN_POINT('Origin',(1.6,0.2,55.));
#7154=CARTESIAN_POINT('Origin',(1.6,0.4,115.));
#7155=CARTESIAN_POINT('',(1.375,0.4,115.));
#7156=CARTESIAN_POINT('Origin',(1.6,0.4,115.));
#7157=CARTESIAN_POINT('',(1.375,0.2,115.));
#7158=CARTESIAN_POINT('',(1.375,0.4,115.));
#7159=CARTESIAN_POINT('Origin',(1.6,0.2,115.));
#7160=CARTESIAN_POINT('Origin',(0.,0.,113.323333333333));
#7161=CARTESIAN_POINT('',(0.369323706252388,0.2,113.323333333333));
#7162=CARTESIAN_POINT('',(0.25,0.2,113.323333333333));
#7163=CARTESIAN_POINT('',(0.125,0.2,113.323333333333));
#7164=CARTESIAN_POINT('',(0.25,0.337490740613724,113.323333333333));
#7165=CARTESIAN_POINT('Origin',(0.,0.,113.323333333333));
#7166=CARTESIAN_POINT('',(0.25,0.2,113.323333333333));
#7167=CARTESIAN_POINT('Origin',(0.,0.,113.323333333333));
#7168=CARTESIAN_POINT('',(0.369323706252388,0.2,170.));
#7169=CARTESIAN_POINT('',(0.369323706252388,0.2,113.323333333333));
#7170=CARTESIAN_POINT('',(0.25,0.337490740613724,170.));
#7171=CARTESIAN_POINT('Origin',(0.,0.,170.));
#7172=CARTESIAN_POINT('',(0.25,0.337490740613724,113.323333333333));
#7173=CARTESIAN_POINT('Origin',(0.25,0.2,0.));
#7174=CARTESIAN_POINT('',(0.25,0.2,113.313333333333));
#7175=CARTESIAN_POINT('',(0.25,0.2,0.));
#7176=CARTESIAN_POINT('',(0.346410161513776,0.2,113.313333333333));
#7177=CARTESIAN_POINT('',(0.125,0.2,113.313333333333));
#7178=CARTESIAN_POINT('',(0.346410161513776,0.2,56.6866666666667));
#7179=CARTESIAN_POINT('',(0.346410161513776,0.2,56.6866666666667));
#7180=CARTESIAN_POINT('',(0.25,0.2,56.6866666666667));
#7181=CARTESIAN_POINT('',(0.125,0.2,56.6866666666667));
#7182=CARTESIAN_POINT('',(0.25,0.2,56.6766666666667));
#7183=CARTESIAN_POINT('',(0.25,0.2,0.));
#7184=CARTESIAN_POINT('',(0.369323706252388,0.2,56.6766666666667));
#7185=CARTESIAN_POINT('',(0.125,0.2,56.6766666666667));
#7186=CARTESIAN_POINT('',(0.369323706252388,0.2,0.));
#7187=CARTESIAN_POINT('',(0.369323706252388,0.2,0.));
#7188=CARTESIAN_POINT('',(2.7,0.2,0.));
#7189=CARTESIAN_POINT('',(0.25,0.2,0.));
#7190=CARTESIAN_POINT('',(2.7,0.2,170.));
#7191=CARTESIAN_POINT('',(2.7,0.2,0.));
#7192=CARTESIAN_POINT('',(0.25,0.2,170.));
#7193=CARTESIAN_POINT('Origin',(0.25,0.4,0.));
#7194=CARTESIAN_POINT('',(0.25,0.4,170.));
#7195=CARTESIAN_POINT('',(0.25,0.4,170.));
#7196=CARTESIAN_POINT('',(0.25,0.4,0.));
#7197=CARTESIAN_POINT('',(0.25,0.4,0.));
#7198=CARTESIAN_POINT('',(0.25,0.337490740613724,0.));
#7199=CARTESIAN_POINT('',(0.25,0.4,0.));
#7200=CARTESIAN_POINT('',(0.25,0.337490740613724,56.6766666666667));
#7201=CARTESIAN_POINT('',(0.25,0.337490740613724,0.));
#7202=CARTESIAN_POINT('',(0.25,0.2,56.6766666666667));
#7203=CARTESIAN_POINT('',(0.25,0.31224989991992,56.6866666666667));
#7204=CARTESIAN_POINT('',(0.25,0.2,56.6866666666667));
#7205=CARTESIAN_POINT('',(0.25,0.31224989991992,113.313333333333));
#7206=CARTESIAN_POINT('',(0.25,0.31224989991992,56.6866666666667));
#7207=CARTESIAN_POINT('',(0.25,0.2,113.313333333333));
#7208=CARTESIAN_POINT('Origin',(0.,0.,0.));
#7209=CARTESIAN_POINT('Origin',(0.,0.,56.6766666666667));
#7210=CARTESIAN_POINT('Origin',(0.,0.,0.));
#7211=CARTESIAN_POINT('Origin',(0.,0.,56.6766666666667));
#7212=CARTESIAN_POINT('Origin',(1.475,0.3,0.));
#7213=CARTESIAN_POINT('',(2.7,0.4,0.));
#7214=CARTESIAN_POINT('',(2.7,0.4,0.));
#7215=CARTESIAN_POINT('',(2.7,0.2,0.));
#7216=CARTESIAN_POINT('Origin',(0.,0.,113.313333333333));
#7217=CARTESIAN_POINT('Origin',(0.,0.,113.313333333333));
#7218=CARTESIAN_POINT('',(-0.22,-2.69422295812418E-17,113.313333333333));
#7219=CARTESIAN_POINT('Origin',(0.,0.,113.313333333333));
#7220=CARTESIAN_POINT('Origin',(0.,0.,56.6866666666667));
#7221=CARTESIAN_POINT('',(-0.22,-2.69422295812418E-17,56.6866666666667));
#7222=CARTESIAN_POINT('',(-0.22,-2.69422295812418E-17,56.6866666666667));
#7223=CARTESIAN_POINT('Origin',(0.,0.,56.6866666666667));
#7224=CARTESIAN_POINT('Origin',(0.,0.,56.6866666666667));
#7225=CARTESIAN_POINT('Origin',(0.,0.,56.6866666666667));
#7226=CARTESIAN_POINT('Origin',(0.,0.,56.6866666666667));
#7227=CARTESIAN_POINT('Origin',(2.7,0.4,0.));
#7228=CARTESIAN_POINT('',(2.7,0.4,170.));
#7229=CARTESIAN_POINT('',(2.7,0.4,170.));
#7230=CARTESIAN_POINT('',(2.7,0.4,0.));
#7231=CARTESIAN_POINT('Origin',(2.7,0.2,0.));
#7232=CARTESIAN_POINT('',(2.7,0.2,170.));
#7233=CARTESIAN_POINT('Origin',(1.475,0.3,170.));
#7234=CARTESIAN_POINT('',(0.,0.,0.));
#7235=CARTESIAN_POINT('Origin',(0.,0.,170.));
#7236=CARTESIAN_POINT('',(-0.3,-3.67394039744206E-17,170.));
#7237=CARTESIAN_POINT('Origin',(0.,0.,170.));
#7238=CARTESIAN_POINT('',(-0.2,2.44929359829471E-17,170.));
#7239=CARTESIAN_POINT('Origin',(0.,0.,170.));
#7240=CARTESIAN_POINT('Origin',(0.,0.,170.));
#7241=CARTESIAN_POINT('',(-0.3,-3.67394039744206E-17,170.2));
#7242=CARTESIAN_POINT('Origin',(0.,0.,170.2));
#7243=CARTESIAN_POINT('',(-0.3,-3.67394039744206E-17,170.));
#7244=CARTESIAN_POINT('Origin',(0.,0.,0.));
#7245=CARTESIAN_POINT('',(-0.35,-4.28626379701574E-17,0.));
#7246=CARTESIAN_POINT('Origin',(0.,0.,0.));
#7247=CARTESIAN_POINT('',(-0.2,-2.44929359829471E-17,0.));
#7248=CARTESIAN_POINT('Origin',(0.,0.,0.));
#7249=CARTESIAN_POINT('Origin',(0.,0.,-0.2));
#7250=CARTESIAN_POINT('',(-0.35,-4.28626379701574E-17,-0.2));
#7251=CARTESIAN_POINT('',(-0.35,-4.28626379701574E-17,-0.2));
#7252=CARTESIAN_POINT('Origin',(0.,0.,-0.2));
#7253=CARTESIAN_POINT('Origin',(0.,0.,-0.2));
#7254=CARTESIAN_POINT('Origin',(0.,0.,0.));
#7255=CARTESIAN_POINT('',(-0.2,-2.44929359829471E-17,0.));
#7256=CARTESIAN_POINT('Origin',(0.,0.,170.2));
#7257=CARTESIAN_POINT('',(0.,0.,0.));
#7258=CARTESIAN_POINT('Origin',(0.,0.,0.));
#7259=CARTESIAN_POINT('',(-0.195635777923873,0.00012637639400136,0.022586969212423));
#7260=CARTESIAN_POINT('',(-0.195586996729399,0.000207538314137144,0.0124130307875798));
#7261=CARTESIAN_POINT('',(-0.1954,-2.39295984553393E-17,0.));
#7262=CARTESIAN_POINT('',(0.0861525859670519,0.175382131162755,0.));
#7263=CARTESIAN_POINT('Ctrl Pts',(-0.195635777923873,0.00012637639400136,
0.022586969212423));
#7264=CARTESIAN_POINT('Ctrl Pts',(-0.195681347828373,0.00674175378970602,
0.0222084605749147));
#7265=CARTESIAN_POINT('Ctrl Pts',(-0.195374969862562,0.0133525801096144,
0.0218299519374064));
#7266=CARTESIAN_POINT('Ctrl Pts',(-0.194702755071016,0.0199256447333511,
0.0214514432998981));
#7267=CARTESIAN_POINT('Ctrl Pts',(-0.188123007026072,0.0842638736018979,
0.0177465390059727));
#7268=CARTESIAN_POINT('Ctrl Pts',(-0.146493114019884,0.144984224685349,
0.0140416347120473));
#7269=CARTESIAN_POINT('Ctrl Pts',(-0.0888552784097874,0.174368623359793,
0.0103367304181219));
#7270=CARTESIAN_POINT('Ctrl Pts',(-0.03525184529165,0.201696239540897,0.00689115361208129));
#7271=CARTESIAN_POINT('Ctrl Pts',(0.0321969844649043,0.201921141720556,
0.00344557680604065));
#7272=CARTESIAN_POINT('Ctrl Pts',(0.0863566694936594,0.175642871684081,
1.97324795392362E-17));
#7273=CARTESIAN_POINT('',(-0.0861525859670424,0.175382131162759,0.));
#7274=CARTESIAN_POINT('Origin',(0.,0.,0.));
#7275=CARTESIAN_POINT('Ctrl Pts',(-0.0861525859670425,0.175382131162759,
-6.38378239159465E-16));
#7276=CARTESIAN_POINT('Ctrl Pts',(-0.14447616479259,0.146731965348487,0.00370490429392476));
#7277=CARTESIAN_POINT('Ctrl Pts',(-0.18688174608519,0.0869523829547151,
0.00740980858785015));
#7278=CARTESIAN_POINT('Ctrl Pts',(-0.194371679194925,0.0228123128668349,
0.0111147128817756));
#7279=CARTESIAN_POINT('Ctrl Pts',(-0.195246583870653,0.0153200634169035,
0.0115474855170436));
#7280=CARTESIAN_POINT('Ctrl Pts',(-0.195645073240692,0.00776831620061643,
0.0119802581523117));
#7281=CARTESIAN_POINT('Ctrl Pts',(-0.195586996729399,0.000207538314137144,
0.0124130307875798));
#7282=CARTESIAN_POINT('Origin',(0.,0.,0.));
#7283=CARTESIAN_POINT('',(-0.195131096902049,0.000101113969644753,0.092586969212423));
#7284=CARTESIAN_POINT('',(-0.195116749400228,8.89926274127593E-5,0.0824130307875797));
#7285=CARTESIAN_POINT('',(-0.1954,-2.39295984553393E-17,0.));
#7286=CARTESIAN_POINT('Ctrl Pts',(-0.195131096902049,0.000101113969644753,
0.092586969212423));
#7287=CARTESIAN_POINT('Ctrl Pts',(-0.195253097178586,0.026184219880761,
0.0911045530051337));
#7288=CARTESIAN_POINT('Ctrl Pts',(-0.190391876856765,0.0522236645961475,
0.0896221367978444));
#7289=CARTESIAN_POINT('Ctrl Pts',(-0.180332593264173,0.0760702837060908,
0.0881397205905551));
#7290=CARTESIAN_POINT('Ctrl Pts',(-0.155192094399714,0.135668553815123,
0.0844348162966297));
#7291=CARTESIAN_POINT('Ctrl Pts',(-0.0975836177799518,0.181570066253063,
0.0807299120027044));
#7292=CARTESIAN_POINT('Ctrl Pts',(-0.0338757516333478,0.192766106246862,
0.077025007708779));
#7293=CARTESIAN_POINT('Ctrl Pts',(0.029832114513256,0.203962146240662,0.0733201034148536));
#7294=CARTESIAN_POINT('Ctrl Pts',(0.0996393701867018,0.180452713790321,
0.0696151991209281));
#7295=CARTESIAN_POINT('Ctrl Pts',(0.143592949422358,0.132995684060219,0.0659102948270027));
#7296=CARTESIAN_POINT('Ctrl Pts',(0.187546528658014,0.0855386543301167,
0.0622053905330773));
#7297=CARTESIAN_POINT('Ctrl Pts',(0.205646431455881,0.0141340273202524,
0.058500486239152));
#7298=CARTESIAN_POINT('Ctrl Pts',(0.189608855488219,-0.0485288059909611,
0.0547955819452266));
#7299=CARTESIAN_POINT('Ctrl Pts',(0.173571279520558,-0.111191639302175,
0.0510906776513013));
#7300=CARTESIAN_POINT('Ctrl Pts',(0.123396224787368,-0.165112678914738,
0.0473857733573758));
#7301=CARTESIAN_POINT('Ctrl Pts',(0.0620482175311841,-0.185621711873549,
0.0436808690634505));
#7302=CARTESIAN_POINT('Ctrl Pts',(0.000700210274999877,-0.206130744832361,
0.0399759647695251));
#7303=CARTESIAN_POINT('Ctrl Pts',(-0.0718207495041789,-0.193227771137421,
0.0362710604755997));
#7304=CARTESIAN_POINT('Ctrl Pts',(-0.122316427851919,-0.15279823096313,
0.0325661561816743));
#7305=CARTESIAN_POINT('Ctrl Pts',(-0.167653254878506,-0.116499143009035,
0.0292397605252572));
#7306=CARTESIAN_POINT('Ctrl Pts',(-0.19523530216884,-0.0580106393937795,
0.0259133648688401));
#7307=CARTESIAN_POINT('Ctrl Pts',(-0.195635777923873,0.00012637639400136,
0.022586969212423));
#7308=CARTESIAN_POINT('Ctrl Pts',(-0.195586996729399,0.000207538314137144,
0.0124130307875798));
#7309=CARTESIAN_POINT('Ctrl Pts',(-0.195147888579442,-0.056958415977544,
0.0156851624462371));
#7310=CARTESIAN_POINT('Ctrl Pts',(-0.168608485816707,-0.114640622495256,
0.0189572941048945));
#7311=CARTESIAN_POINT('Ctrl Pts',(-0.124548266143515,-0.151025787390765,
0.0222294257635518));
#7312=CARTESIAN_POINT('Ctrl Pts',(-0.0746606350555016,-0.192223259778496,
0.0259343300574772));
#7313=CARTESIAN_POINT('Ctrl Pts',(-0.00231108795260535,-0.20611764677197,
0.0296392343514025));
#7314=CARTESIAN_POINT('Ctrl Pts',(0.0593359806590351,-0.186491079647165,
0.0333441386453279));
#7315=CARTESIAN_POINT('Ctrl Pts',(0.120983049270676,-0.16686451252236,0.0370490429392533));
#7316=CARTESIAN_POINT('Ctrl Pts',(0.17192763939106,-0.113716991279275,0.0407539472331787));
#7317=CARTESIAN_POINT('Ctrl Pts',(0.188876026712615,-0.0513034241454011,
0.0444588515271041));
#7318=CARTESIAN_POINT('Ctrl Pts',(0.205824414034169,0.0111101429884734,
0.0481637558210295));
#7319=CARTESIAN_POINT('Ctrl Pts',(0.188776598556893,0.082789756013138,0.0518686601149549));
#7320=CARTESIAN_POINT('Ctrl Pts',(0.14552275371934,0.130888260289707,0.0555735644088803));
#7321=CARTESIAN_POINT('Ctrl Pts',(0.102268908881787,0.178986764566276,0.0592784687028057));
#7322=CARTESIAN_POINT('Ctrl Pts',(0.0328090346839575,0.203504160094748,
0.0629833729967312));
#7323=CARTESIAN_POINT('Ctrl Pts',(-0.0310564735112635,0.193237932504459,
0.0666882772906565));
#7324=CARTESIAN_POINT('Ctrl Pts',(-0.0949219817064845,0.18297170491417,
0.0703931815845819));
#7325=CARTESIAN_POINT('Ctrl Pts',(-0.153193123899096,0.137921854205119,
0.0740980858785072));
#7326=CARTESIAN_POINT('Ctrl Pts',(-0.179201322195063,0.0786984774853335,
0.0778029901724326));
#7327=CARTESIAN_POINT('Ctrl Pts',(-0.189988721900888,0.0541344446624959,
0.0793396703774816));
#7328=CARTESIAN_POINT('Ctrl Pts',(-0.195225814685876,0.0271320906572496,
0.0808763505825307));
#7329=CARTESIAN_POINT('Ctrl Pts',(-0.195116749400228,8.89926274127593E-5,
0.0824130307875797));
#7330=CARTESIAN_POINT('Origin',(0.,0.,0.));
#7331=CARTESIAN_POINT('',(-0.195269961073647,-0.00016635217456426,0.162586969212423));
#7332=CARTESIAN_POINT('',(-0.195296072527608,-0.000171556393799694,0.15241303078758));
#7333=CARTESIAN_POINT('',(-0.1954,-2.39295984553393E-17,0.));
#7334=CARTESIAN_POINT('Ctrl Pts',(-0.195269961073647,-0.00016635217456426,
0.162586969212423));
#7335=CARTESIAN_POINT('Ctrl Pts',(-0.194902238792413,0.0452585421341261,
0.160000645435353));
#7336=CARTESIAN_POINT('Ctrl Pts',(-0.179109205182361,0.0909139814220055,
0.157414321658282));
#7337=CARTESIAN_POINT('Ctrl Pts',(-0.150142749348677,0.125553440155619,
0.154827997881212));
#7338=CARTESIAN_POINT('Ctrl Pts',(-0.108648351953627,0.175174404297546,
0.151123093587287));
#7339=CARTESIAN_POINT('Ctrl Pts',(-0.0401214170626077,0.202190011810589,
0.147418189293361));
#7340=CARTESIAN_POINT('Ctrl Pts',(0.0240715464793194,0.194234567703968,
0.143713284999436));
#7341=CARTESIAN_POINT('Ctrl Pts',(0.0882645100212464,0.186279123597346,
0.140008380705511));
#7342=CARTESIAN_POINT('Ctrl Pts',(0.148123502214081,0.143352627871059,0.136303476411585));
#7343=CARTESIAN_POINT('Ctrl Pts',(0.176249534614617,0.0851035623277452,
0.13259857211766));
#7344=CARTESIAN_POINT('Ctrl Pts',(0.204375567015153,0.0268544967844316,
0.128893667823734));
#7345=CARTESIAN_POINT('Ctrl Pts',(0.20076863962339,-0.0467171385759083,
0.125188763529809));
#7346=CARTESIAN_POINT('Ctrl Pts',(0.167079755224462,-0.101935622009865,
0.121483859235884));
#7347=CARTESIAN_POINT('Ctrl Pts',(0.133390870825534,-0.157154105443821,
0.117778954941958));
#7348=CARTESIAN_POINT('Ctrl Pts',(0.0696200294194389,-0.194019436951393,
0.114074050648033));
#7349=CARTESIAN_POINT('Ctrl Pts',(0.00495672165634356,-0.195657648289217,
0.110369146354107));
#7350=CARTESIAN_POINT('Ctrl Pts',(-0.0597065861067518,-0.19729585962704,
0.106664242060182));
#7351=CARTESIAN_POINT('Ctrl Pts',(-0.125262360226848,-0.163706950795115,
0.102959337766257));
#7352=CARTESIAN_POINT('Ctrl Pts',(-0.161703986732318,-0.11026498248909,
0.0992544334723314));
#7353=CARTESIAN_POINT('Ctrl Pts',(-0.183564492251676,-0.0782063573631269,
0.0970319453856953));
#7354=CARTESIAN_POINT('Ctrl Pts',(-0.19494818999653,-0.0390035530360715,
0.0948094572990591));
#7355=CARTESIAN_POINT('Ctrl Pts',(-0.195131096902049,0.000101113969644753,
0.092586969212423));
#7356=CARTESIAN_POINT('Ctrl Pts',(-0.195116749400228,8.89926274127593E-5,
0.0824130307875797));
#7357=CARTESIAN_POINT('Ctrl Pts',(-0.194962860530686,-0.0380682611678014,
0.0845812548764561));
#7358=CARTESIAN_POINT('Ctrl Pts',(-0.184165504319832,-0.0763066307267761,
0.0867494789653325));
#7359=CARTESIAN_POINT('Ctrl Pts',(-0.163298148442827,-0.10789116262043,
0.0889177030542089));
#7360=CARTESIAN_POINT('Ctrl Pts',(-0.127641521995304,-0.161860523275888,
0.0926226073481343));
#7361=CARTESIAN_POINT('Ctrl Pts',(-0.0625830147009374,-0.196402341856286,
0.0963275116420596));
#7362=CARTESIAN_POINT('Ctrl Pts',(0.00209745128795896,-0.195708815241575,
0.100032415935985));
#7363=CARTESIAN_POINT('Ctrl Pts',(0.0667779172768549,-0.195015288626865,
0.10373732022991));
#7364=CARTESIAN_POINT('Ctrl Pts',(0.13108034196028,-0.159086416817049,0.107442224523836));
#7365=CARTESIAN_POINT('Ctrl Pts',(0.165572399043018,-0.104366250199005,
0.111147128817761));
#7366=CARTESIAN_POINT('Ctrl Pts',(0.200064456125757,-0.0496460835809611,
0.114852033111687));
#7367=CARTESIAN_POINT('Ctrl Pts',(0.204746145607807,0.0238653778453102,
0.118556937405612));
#7368=CARTESIAN_POINT('Ctrl Pts',(0.177474264716175,0.0825192844773609,
0.122261841699537));
#7369=CARTESIAN_POINT('Ctrl Pts',(0.150202383824543,0.141173191109411,0.125966745993463));
#7370=CARTESIAN_POINT('Ctrl Pts',(0.0909769325592305,0.184969542947241,
0.129671650287388));
#7371=CARTESIAN_POINT('Ctrl Pts',(0.0269070452168959,0.193862055706153,
0.133376554581313));
#7372=CARTESIAN_POINT('Ctrl Pts',(-0.037162842125439,0.202754568465066,
0.137081458875239));
#7373=CARTESIAN_POINT('Ctrl Pts',(-0.106077165544796,0.176743242145061,
0.140786363169164));
#7374=CARTESIAN_POINT('Ctrl Pts',(-0.148292168871142,0.127733901391228,
0.14449126746309));
#7375=CARTESIAN_POINT('Ctrl Pts',(-0.178379969487403,0.0928035885463768,
0.14713185523792));
#7376=CARTESIAN_POINT('Ctrl Pts',(-0.194905030259773,0.0461907277712621,
0.14977244301275));
#7377=CARTESIAN_POINT('Ctrl Pts',(-0.195296072527608,-0.000171556393799694,
0.15241303078758));
#7378=CARTESIAN_POINT('Origin',(0.,0.,0.));
#7379=CARTESIAN_POINT('',(-0.195720342430618,-4.78848216406425E-6,0.232586969212423));
#7380=CARTESIAN_POINT('',(-0.195719426634615,1.29078158682454E-5,0.22241303078758));
#7381=CARTESIAN_POINT('',(-0.1954,-2.39295984553393E-17,0.));
#7382=CARTESIAN_POINT('Ctrl Pts',(-0.195720342430618,-4.78848216406425E-6,
0.232586969212423));
#7383=CARTESIAN_POINT('Ctrl Pts',(-0.195697143051313,0.0644232125710103,
0.228896737865572));
#7384=CARTESIAN_POINT('Ctrl Pts',(-0.160777086274134,0.128872764270736,
0.22520650651872));
#7385=CARTESIAN_POINT('Ctrl Pts',(-0.106783173118586,0.164023975286507,
0.221516275171869));
#7386=CARTESIAN_POINT('Ctrl Pts',(-0.0525745715720951,0.199314953111009,
0.217811370877944));
#7387=CARTESIAN_POINT('Ctrl Pts',(0.0208598692839071,0.205074137319626,
0.214106466584018));
#7388=CARTESIAN_POINT('Ctrl Pts',(0.0799073451636341,0.178665404061868,
0.210401562290093));
#7389=CARTESIAN_POINT('Ctrl Pts',(0.138954821043361,0.152256670804111,0.206696657996168));
#7390=CARTESIAN_POINT('Ctrl Pts',(0.183615331946813,0.0936800200799801,
0.202991753702242));
#7391=CARTESIAN_POINT('Ctrl Pts',(0.193446630107478,0.0297474679262876,
0.199286849408317));
#7392=CARTESIAN_POINT('Ctrl Pts',(0.203277928268144,-0.0341850842274047,
0.195581945114392));
#7393=CARTESIAN_POINT('Ctrl Pts',(0.178280013686022,-0.103473537810658,
0.191877040820466));
#7394=CARTESIAN_POINT('Ctrl Pts',(0.129895065749049,-0.146402809319959,
0.188172136526541));
#7395=CARTESIAN_POINT('Ctrl Pts',(0.0815101178120762,-0.18933208082926,
0.184467232232615));
#7396=CARTESIAN_POINT('Ctrl Pts',(0.00973813652025106,-0.205902170264609,
0.18076232793869));
#7397=CARTESIAN_POINT('Ctrl Pts',(-0.0525690244207131,-0.188528532620279,
0.177057423644765));
#7398=CARTESIAN_POINT('Ctrl Pts',(-0.114876185361677,-0.171154894975948,
0.173352519350839));
#7399=CARTESIAN_POINT('Ctrl Pts',(-0.16771852595178,-0.119837530251938,
0.169647615056914));
#7400=CARTESIAN_POINT('Ctrl Pts',(-0.186908766297293,-0.0580656875045278,
0.165942710762988));
#7401=CARTESIAN_POINT('Ctrl Pts',(-0.192702661972129,-0.0394156025615012,
0.164824130246133));
#7402=CARTESIAN_POINT('Ctrl Pts',(-0.195429000318094,-0.0198125396335311,
0.163705549729278));
#7403=CARTESIAN_POINT('Ctrl Pts',(-0.195269961073647,-0.00016635217456426,
0.162586969212423));
#7404=CARTESIAN_POINT('Ctrl Pts',(-0.195296072527608,-0.000171556393799694,
0.15241303078758));
#7405=CARTESIAN_POINT('Ctrl Pts',(-0.195453686203354,-0.0188583599040719,
0.153477347306675));
#7406=CARTESIAN_POINT('Ctrl Pts',(-0.192990203806021,-0.0375044553062908,
0.15454166382577));
#7407=CARTESIAN_POINT('Ctrl Pts',(-0.187737257267333,-0.0553284581639518,
0.155605980344866));
#7408=CARTESIAN_POINT('Ctrl Pts',(-0.169451659103841,-0.117374121777638,
0.159310884638791));
#7409=CARTESIAN_POINT('Ctrl Pts',(-0.117364779543521,-0.169458093817348,
0.163015788932717));
#7410=CARTESIAN_POINT('Ctrl Pts',(-0.0553181242256267,-0.187740280857214,
0.166720693226642));
#7411=CARTESIAN_POINT('Ctrl Pts',(0.00672853109226811,-0.20602246789708,
0.170425597520567));
#7412=CARTESIAN_POINT('Ctrl Pts',(0.0787349621677377,-0.190502869937101,
0.174130501814493));
#7413=CARTESIAN_POINT('Ctrl Pts',(0.127742011886824,-0.148285168489488,
0.177835406108418));
#7414=CARTESIAN_POINT('Ctrl Pts',(0.17674906160591,-0.106067467041874,0.181540310402344));
#7415=CARTESIAN_POINT('Ctrl Pts',(0.202756729968613,-0.0371516621066246,
0.185245214696269));
#7416=CARTESIAN_POINT('Ctrl Pts',(0.193860642333605,0.0269177193885033,
0.188950118990194));
#7417=CARTESIAN_POINT('Ctrl Pts',(0.184964554698597,0.0909871008836312,
0.19265502328412));
#7418=CARTESIAN_POINT('Ctrl Pts',(0.141164711065879,0.150210058938638,0.196359927578045));
#7419=CARTESIAN_POINT('Ctrl Pts',(0.0825094128007834,0.17747875371355,0.200064831871971));
#7420=CARTESIAN_POINT('Ctrl Pts',(0.0238541145356881,0.204747448488462,
0.203769736165896));
#7421=CARTESIAN_POINT('Ctrl Pts',(-0.0496566383617833,0.200061879983279,
0.207474640459821));
#7422=CARTESIAN_POINT('Ctrl Pts',(-0.104375113131947,0.165566747025073,
0.211179544753747));
#7423=CARTESIAN_POINT('Ctrl Pts',(-0.15909358790211,0.131071614066866,0.214884449047672));
#7424=CARTESIAN_POINT('Ctrl Pts',(-0.195019784544964,0.0667669166556367,
0.218589353341598));
#7425=CARTESIAN_POINT('Ctrl Pts',(-0.195709371646085,0.00208654669905255,
0.222294257635523));
#7426=CARTESIAN_POINT('Ctrl Pts',(-0.195716740656376,0.00139536452478984,
0.222333848686209));
#7427=CARTESIAN_POINT('Ctrl Pts',(-0.195720085887096,0.000704139451294379,
0.222373439736894));
#7428=CARTESIAN_POINT('Ctrl Pts',(-0.195719426634615,1.29078158682454E-5,
0.22241303078758));
#7429=CARTESIAN_POINT('Origin',(0.,0.,0.));
#7430=CARTESIAN_POINT('',(-0.195283952697599,0.000169337138534779,0.302586969212423));
#7431=CARTESIAN_POINT('',(-0.195258340825392,0.000163515663356278,0.29241303078758));
#7432=CARTESIAN_POINT('',(-0.1954,-2.39295984553393E-17,0.));
#7433=CARTESIAN_POINT('Ctrl Pts',(-0.195283952697599,0.000169337138534779,
0.302586969212423));
#7434=CARTESIAN_POINT('Ctrl Pts',(-0.19544242560897,0.0192966383326108,
0.301497734589716));
#7435=CARTESIAN_POINT('Ctrl Pts',(-0.192859982037008,0.0383820720800439,
0.300408499967009));
#7436=CARTESIAN_POINT('Ctrl Pts',(-0.187361774489973,0.0565868885747682,
0.299319265344303));
#7437=CARTESIAN_POINT('Ctrl Pts',(-0.16866026397493,0.11850844467975,0.295614361050377));
#7438=CARTESIAN_POINT('Ctrl Pts',(-0.116225092311322,0.170241781073389,
0.291909456756452));
#7439=CARTESIAN_POINT('Ctrl Pts',(-0.0540571662767995,0.188107238759169,
0.288204552462526));
#7440=CARTESIAN_POINT('Ctrl Pts',(0.00811075975772279,0.205972696444949,
0.284499648168601));
#7441=CARTESIAN_POINT('Ctrl Pts',(0.080011440163159,0.189970275422869,0.280794743874676));
#7442=CARTESIAN_POINT('Ctrl Pts',(0.128734111559132,0.147424689310423,0.27708983958075));
#7443=CARTESIAN_POINT('Ctrl Pts',(0.177456782955104,0.104879103197978,0.273384935286825));
#7444=CARTESIAN_POINT('Ctrl Pts',(0.203001445341614,0.0357903519951666,
0.269680030992899));
#7445=CARTESIAN_POINT('Ctrl Pts',(0.193675659438429,-0.0282178921934112,
0.265975126698974));
#7446=CARTESIAN_POINT('Ctrl Pts',(0.184349873535243,-0.0922261363819893,
0.262270222405049));
#7447=CARTESIAN_POINT('Ctrl Pts',(0.140153639342363,-0.151153873556334,
0.258565318111123));
#7448=CARTESIAN_POINT('Ctrl Pts',(0.081316693190513,-0.178028385131025,
0.254860413817198));
#7449=CARTESIAN_POINT('Ctrl Pts',(0.0224797470386625,-0.204902896705717,
0.251155509523273));
#7450=CARTESIAN_POINT('Ctrl Pts',(-0.0509979110721584,-0.199724182680755,
0.247450605229347));
#7451=CARTESIAN_POINT('Ctrl Pts',(-0.105483695120245,-0.164862671795436,
0.243745700935422));
#7452=CARTESIAN_POINT('Ctrl Pts',(-0.160185265316152,-0.129863094967365,
0.240026123694422));
#7453=CARTESIAN_POINT('Ctrl Pts',(-0.19574372629877,-0.0649451415050078,
0.236306546453423));
#7454=CARTESIAN_POINT('Ctrl Pts',(-0.195720342430618,-4.78848216406425E-6,
0.232586969212423));
#7455=CARTESIAN_POINT('Ctrl Pts',(-0.195719426634615,1.29078158682454E-5,
0.22241303078758));
#7456=CARTESIAN_POINT('Ctrl Pts',(-0.195658393476725,-0.0639808590481945,
0.22607834403082));
#7457=CARTESIAN_POINT('Ctrl Pts',(-0.161275200187356,-0.128030867785169,
0.229743657274059));
#7458=CARTESIAN_POINT('Ctrl Pts',(-0.107881352358607,-0.163303782908962,
0.233408970517299));
#7459=CARTESIAN_POINT('Ctrl Pts',(-0.0539107684106243,-0.198957700058453,
0.237113874811225));
#7460=CARTESIAN_POINT('Ctrl Pts',(0.0194833770447268,-0.205209491855498,
0.24081877910515));
#7461=CARTESIAN_POINT('Ctrl Pts',(0.0787067240594876,-0.179197554104805,
0.244523683399075));
#7462=CARTESIAN_POINT('Ctrl Pts',(0.137930071074249,-0.153185616354111,
0.248228587693001));
#7463=CARTESIAN_POINT('Ctrl Pts',(0.182982619648419,-0.0949099490556798,
0.251933491986926));
#7464=CARTESIAN_POINT('Ctrl Pts',(0.193242676546893,-0.0310448021878294,
0.255638396280851));
#7465=CARTESIAN_POINT('Ctrl Pts',(0.203502733445366,0.0328203446800207,
0.259343300574777));
#7466=CARTESIAN_POINT('Ctrl Pts',(0.178970298668143,0.10227497111729,0.263048204868703));
#7467=CARTESIAN_POINT('Ctrl Pts',(0.130874489328304,0.145527934810222,0.266753109162628));
#7468=CARTESIAN_POINT('Ctrl Pts',(0.0827786799884639,0.188780898503155,
0.270458013456553));
#7469=CARTESIAN_POINT('Ctrl Pts',(0.0111194960860082,0.205832199451752,
0.274162917750478));
#7470=CARTESIAN_POINT('Ctrl Pts',(-0.0513028380988605,0.188877025035076,
0.277867822044404));
#7471=CARTESIAN_POINT('Ctrl Pts',(-0.113725172283729,0.1719218506184,0.281572726338329));
#7472=CARTESIAN_POINT('Ctrl Pts',(-0.166910656751011,0.120960200836452,
0.285277630632255));
#7473=CARTESIAN_POINT('Ctrl Pts',(-0.186514947523482,0.0593185142124166,
0.28898253492618));
#7474=CARTESIAN_POINT('Ctrl Pts',(-0.192565705566086,0.0402931418881201,
0.290126033546647));
#7475=CARTESIAN_POINT('Ctrl Pts',(-0.195417469557725,0.0202503734988586,
0.291269532167113));
#7476=CARTESIAN_POINT('Ctrl Pts',(-0.195258340825392,0.000163515663356278,
0.29241303078758));
#7477=CARTESIAN_POINT('Origin',(0.,0.,0.));
#7478=CARTESIAN_POINT('',(-0.195123386395527,-9.37244138880245E-5,0.372586969212423));
#7479=CARTESIAN_POINT('',(-0.195138177948142,-0.000106777846584659,0.36241303078758));
#7480=CARTESIAN_POINT('',(-0.1954,-2.39295984553393E-17,0.));
#7481=CARTESIAN_POINT('Ctrl Pts',(-0.195123386395527,-9.37244138880245E-5,
0.372586969212423));
#7482=CARTESIAN_POINT('Ctrl Pts',(-0.19495607068899,0.0384983387935844,
0.370393827019935));
#7483=CARTESIAN_POINT('Ctrl Pts',(-0.183891455427995,0.0771788701751315,
0.368200684827447));
#7484=CARTESIAN_POINT('Ctrl Pts',(-0.162570246636473,0.108983601551862,
0.366007542634959));
#7485=CARTESIAN_POINT('Ctrl Pts',(-0.126552044864621,0.162711757550323,
0.362302638341034));
#7486=CARTESIAN_POINT('Ctrl Pts',(-0.0612637871930766,0.196817896755676,
0.358597734047109));
#7487=CARTESIAN_POINT('Ctrl Pts',(0.00341043643912528,0.195690775004793,
0.354892829753183));
#7488=CARTESIAN_POINT('Ctrl Pts',(0.0680846600713272,0.194563653253909,
0.351187925459258));
#7489=CARTESIAN_POINT('Ctrl Pts',(0.132144849664187,0.158203270546789,0.347483021165333));
#7490=CARTESIAN_POINT('Ctrl Pts',(0.166269033157579,0.103252695419938,0.343778116871407));
#7491=CARTESIAN_POINT('Ctrl Pts',(0.200393216650971,0.0483021202930879,
0.340073212577482));
#7492=CARTESIAN_POINT('Ctrl Pts',(0.204581394044897,-0.0252386472534923,
0.336368308283556));
#7493=CARTESIAN_POINT('Ctrl Pts',(0.176916530417748,-0.0837081343932021,
0.332663403989631));
#7494=CARTESIAN_POINT('Ctrl Pts',(0.149251666790599,-0.142177621532912,
0.328958499695706));
#7495=CARTESIAN_POINT('Ctrl Pts',(0.0897337621423753,-0.185575828265751,
0.32525359540178));
#7496=CARTESIAN_POINT('Ctrl Pts',(0.025605669612909,-0.19403829565955,0.321548691107855));
#7497=CARTESIAN_POINT('Ctrl Pts',(-0.0385224229165574,-0.202500763053348,
0.317843786813929));
#7498=CARTESIAN_POINT('Ctrl Pts',(-0.107260703327267,-0.176027491108105,
0.314138882520004));
#7499=CARTESIAN_POINT('Ctrl Pts',(-0.149145918849381,-0.126735967227322,
0.310433978226078));
#7500=CARTESIAN_POINT('Ctrl Pts',(-0.178716962855371,-0.0919360550475366,
0.30781830855486));
#7501=CARTESIAN_POINT('Ctrl Pts',(-0.194903398518234,-0.0457626416864486,
0.305202638883641));
#7502=CARTESIAN_POINT('Ctrl Pts',(-0.195283952697599,0.000169337138534779,
0.302586969212423));
#7503=CARTESIAN_POINT('Ctrl Pts',(-0.195258340825392,0.000163515663356278,
0.29241303078758));
#7504=CARTESIAN_POINT('Ctrl Pts',(-0.194901896811807,-0.0448304971854093,
0.294974436461039));
#7505=CARTESIAN_POINT('Ctrl Pts',(-0.179438365931039,-0.0900457278440895,
0.297535842134498));
#7506=CARTESIAN_POINT('Ctrl Pts',(-0.150981821407715,-0.124543170751799,
0.300097247807956));
#7507=CARTESIAN_POINT('Ctrl Pts',(-0.109821307441813,-0.174441445625855,
0.303802152101882));
#7508=CARTESIAN_POINT('Ctrl Pts',(-0.0414771824323471,-0.201916271907844,
0.307507056395807));
#7509=CARTESIAN_POINT('Ctrl Pts',(0.0227677157704201,-0.194391725382998,
0.311211960689733));
#7510=CARTESIAN_POINT('Ctrl Pts',(0.0870126139731875,-0.186867178858152,
0.314916864983658));
#7511=CARTESIAN_POINT('Ctrl Pts',(0.147158285369256,-0.14434325952647,0.318621769277583));
#7512=CARTESIAN_POINT('Ctrl Pts',(0.175674532068328,-0.0862842428284894,
0.322326673571509));
#7513=CARTESIAN_POINT('Ctrl Pts',(0.204190778767399,-0.0282252261305095,
0.326031577865434));
#7514=CARTESIAN_POINT('Ctrl Pts',(0.201077600769473,0.0453688879337687,
0.32973648215936));
#7515=CARTESIAN_POINT('Ctrl Pts',(0.167759978533406,0.100812208488104,0.333441386453285));
#7516=CARTESIAN_POINT('Ctrl Pts',(0.134442356297339,0.156255529042441,0.33714629074721));
#7517=CARTESIAN_POINT('Ctrl Pts',(0.070920289823129,0.193548056086834,0.340851195041136));
#7518=CARTESIAN_POINT('Ctrl Pts',(0.00626943858281168,0.195620054999355,
0.344556099335061));
#7519=CARTESIAN_POINT('Ctrl Pts',(-0.0583814126575052,0.197692053911877,
0.348261003628986));
#7520=CARTESIAN_POINT('Ctrl Pts',(-0.12416104866393,0.164543524692526,0.351965907922912));
#7521=CARTESIAN_POINT('Ctrl Pts',(-0.160960463181693,0.111347389148941,
0.355670812216837));
#7522=CARTESIAN_POINT('Ctrl Pts',(-0.18328309972599,0.0790784518611643,
0.357918218407085));
#7523=CARTESIAN_POINT('Ctrl Pts',(-0.19494196408341,0.0394326521564634,
0.360165624597332));
#7524=CARTESIAN_POINT('Ctrl Pts',(-0.195138177948142,-0.000106777846584659,
0.36241303078758));
#7525=CARTESIAN_POINT('Origin',(0.,0.,0.));
#7526=CARTESIAN_POINT('',(-0.195626364086859,-0.000119838590748017,0.442586969212423));
#7527=CARTESIAN_POINT('',(-0.195647655240959,-0.000106560329145428,0.43241303078758));
#7528=CARTESIAN_POINT('',(-0.1954,-2.39295984553393E-17,0.));
#7529=CARTESIAN_POINT('Ctrl Pts',(-0.195626364086859,-0.000119838590748017,
0.442586969212423));
#7530=CARTESIAN_POINT('Ctrl Pts',(-0.195210765908107,0.0575169625739688,
0.439289919450154));
#7531=CARTESIAN_POINT('Ctrl Pts',(-0.168170950548248,0.115492749874537,
0.435992869687885));
#7532=CARTESIAN_POINT('Ctrl Pts',(-0.123518955260722,0.151820875343157,
0.432695819925617));
#7533=CARTESIAN_POINT('Ctrl Pts',(-0.0733433798216494,0.192642894343057,
0.428990915631691));
#7534=CARTESIAN_POINT('Ctrl Pts',(-0.00092876126150717,0.206130234335124,
0.425286011337766));
#7535=CARTESIAN_POINT('Ctrl Pts',(0.0605788945201889,0.186109398036142,
0.421581107043841));
#7536=CARTESIAN_POINT('Ctrl Pts',(0.122086550301885,0.16608856173716,0.417876202749915));
#7537=CARTESIAN_POINT('Ctrl Pts',(0.172687243305135,0.11255954914713,0.41417129845599));
#7538=CARTESIAN_POINT('Ctrl Pts',(0.189219754122116,0.0500239457522927,
0.410466394162064));
#7539=CARTESIAN_POINT('Ctrl Pts',(0.205752264939098,-0.0125116576425448,
0.406761489868139));
#7540=CARTESIAN_POINT('Ctrl Pts',(0.188216593569811,-0.0840538518421897,
0.403056585574214));
#7541=CARTESIAN_POINT('Ctrl Pts',(0.14463926115343,-0.131855961684149,0.399351681280288));
#7542=CARTESIAN_POINT('Ctrl Pts',(0.101061928737049,-0.179658071526109,
0.395646776986363));
#7543=CARTESIAN_POINT('Ctrl Pts',(0.0314429352735729,-0.203720097010384,
0.391941872692437));
#7544=CARTESIAN_POINT('Ctrl Pts',(-0.0323513417852891,-0.193028239341701,
0.388236968398512));
#7545=CARTESIAN_POINT('Ctrl Pts',(-0.096145618844151,-0.182336381673018,
0.384532064104586));
#7546=CARTESIAN_POINT('Ctrl Pts',(-0.154115179498399,-0.136890640851379,
0.380827159810661));
#7547=CARTESIAN_POINT('Ctrl Pts',(-0.179725886889443,-0.0774926840447737,
0.377122255516736));
#7548=CARTESIAN_POINT('Ctrl Pts',(-0.190176169475222,-0.0532557340781358,
0.375610493415298));
#7549=CARTESIAN_POINT('Ctrl Pts',(-0.19523871933882,-0.0266957471979921,
0.374098731313861));
#7550=CARTESIAN_POINT('Ctrl Pts',(-0.195123386395527,-9.37244138880245E-5,
0.372586969212423));
#7551=CARTESIAN_POINT('Ctrl Pts',(-0.195138177948142,-0.000106777846584659,
0.36241303078758));
#7552=CARTESIAN_POINT('Ctrl Pts',(-0.195265427457823,-0.0257490691689222,
0.363870528891258));
#7553=CARTESIAN_POINT('Ctrl Pts',(-0.190571668416256,-0.0513466230859282,
0.365328026994935));
#7554=CARTESIAN_POINT('Ctrl Pts',(-0.180838999481628,-0.0748583198076805,
0.366785525098613));
#7555=CARTESIAN_POINT('Ctrl Pts',(-0.156098928234699,-0.134624151352898,
0.370490429392539));
#7556=CARTESIAN_POINT('Ctrl Pts',(-0.0987995927117393,-0.180912072575515,
0.374195333686464));
#7557=CARTESIAN_POINT('Ctrl Pts',(-0.0351683507451656,-0.192534928996931,
0.37790023798039));
#7558=CARTESIAN_POINT('Ctrl Pts',(0.0284628912214086,-0.204157785418346,
0.381605142274315));
#7559=CARTESIAN_POINT('Ctrl Pts',(0.0984260396315977,-0.181115577038558,
0.38531004656824));
#7560=CARTESIAN_POINT('Ctrl Pts',(0.142697188593653,-0.133955306522111,
0.389014950862166));
#7561=CARTESIAN_POINT('Ctrl Pts',(0.186968337555709,-0.086795036005663,
0.392719855156091));
#7562=CARTESIAN_POINT('Ctrl Pts',(0.205547487069631,-0.0155167033525556,
0.396424759450017));
#7563=CARTESIAN_POINT('Ctrl Pts',(0.189930489607766,0.0472537923908843,
0.400129663743942));
#7564=CARTESIAN_POINT('Ctrl Pts',(0.1743134921459,0.110024288134324,0.403834568037867));
#7565=CARTESIAN_POINT('Ctrl Pts',(0.124500347708247,0.164286946968095,0.407539472331793));
#7566=CARTESIAN_POINT('Ctrl Pts',(0.0632917947676797,0.185204374929584,
0.411244376625718));
#7567=CARTESIAN_POINT('Ctrl Pts',(0.00208324182711199,0.206121802891074,
0.414949280919643));
#7568=CARTESIAN_POINT('Ctrl Pts',(-0.0705207196163706,0.19369399998028,
0.418654185213569));
#7569=CARTESIAN_POINT('Ctrl Pts',(-0.121287416627594,0.153609486509697,
0.422359089507494));
#7570=CARTESIAN_POINT('Ctrl Pts',(-0.167209015877504,0.117350579153232,
0.425710403267523));
#7571=CARTESIAN_POINT('Ctrl Pts',(-0.19526267760737,0.0584620801725425,
0.429061717027551));
#7572=CARTESIAN_POINT('Ctrl Pts',(-0.195647655240959,-0.000106560329145428,
0.43241303078758));
#7573=CARTESIAN_POINT('Origin',(0.,0.,0.));
#7574=CARTESIAN_POINT('',(-0.195488415809582,0.000168817958016994,0.512586969212423));
#7575=CARTESIAN_POINT('',(-0.19545977166257,0.000173536236839715,0.502413030787579));
#7576=CARTESIAN_POINT('',(-0.1954,-2.39295984553393E-17,0.));
#7577=CARTESIAN_POINT('Ctrl Pts',(-0.195488415809582,0.000168817958016994,
0.512586969212423));
#7578=CARTESIAN_POINT('Ctrl Pts',(-0.195599493209505,0.0123590955640317,
0.511890916174299));
#7579=CARTESIAN_POINT('Ctrl Pts',(-0.194557059515437,0.0245304346389609,
0.511194863136174));
#7580=CARTESIAN_POINT('Ctrl Pts',(-0.192292612985525,0.0364700080869448,
0.51049881009805));
#7581=CARTESIAN_POINT('Ctrl Pts',(-0.180239569305636,0.100021166565142,
0.506793905804125));
#7582=CARTESIAN_POINT('Ctrl Pts',(-0.133565088753798,0.157006060936268,
0.503089001510199));
#7583=CARTESIAN_POINT('Ctrl Pts',(-0.0736332638087015,0.181341261050928,
0.499384097216274));
#7584=CARTESIAN_POINT('Ctrl Pts',(-0.0137014388636053,0.205676461165589,
0.495679192922349));
#7585=CARTESIAN_POINT('Ctrl Pts',(0.0594877304747487,0.197361967023783,
0.491974288628423));
#7586=CARTESIAN_POINT('Ctrl Pts',(0.112433706788561,0.160203533283279,0.488269384334498));
#7587=CARTESIAN_POINT('Ctrl Pts',(0.165379683102374,0.123045099542775,0.484564480040572));
#7588=CARTESIAN_POINT('Ctrl Pts',(0.198082466391645,0.0570427262035733,
0.480859575746647));
#7589=CARTESIAN_POINT('Ctrl Pts',(0.195573164057203,-0.00759262795856141,
0.477154671452722));
#7590=CARTESIAN_POINT('Ctrl Pts',(0.193063861722761,-0.0722279821206961,
0.473449767158796));
#7591=CARTESIAN_POINT('Ctrl Pts',(0.155342473764606,-0.135496317105764,
0.469744862864871));
#7592=CARTESIAN_POINT('Ctrl Pts',(0.0996750353101687,-0.168438112773147,
0.466039958570945));
#7593=CARTESIAN_POINT('Ctrl Pts',(0.0440075968557312,-0.201379908440531,
0.46233505427702));
#7594=CARTESIAN_POINT('Ctrl Pts',(-0.0296058920949886,-0.20399516479023,
0.458630149983094));
#7595=CARTESIAN_POINT('Ctrl Pts',(-0.0874706722853638,-0.17508681272046,
0.454925245689169));
#7596=CARTESIAN_POINT('Ctrl Pts',(-0.14533545247574,-0.146178460650689,
0.451220341395244));
#7597=CARTESIAN_POINT('Ctrl Pts',(-0.18745152390577,-0.0857465001614493,
0.447515437101318));
#7598=CARTESIAN_POINT('Ctrl Pts',(-0.194541293461784,-0.0214521709129621,
0.443810532807393));
#7599=CARTESIAN_POINT('Ctrl Pts',(-0.195321771015971,-0.014374327205417,
0.443402678275736));
#7600=CARTESIAN_POINT('Ctrl Pts',(-0.195677774776043,-0.00724967654898506,
0.44299482374408));
#7601=CARTESIAN_POINT('Ctrl Pts',(-0.195626364086859,-0.000119838590748017,
0.442586969212423));
#7602=CARTESIAN_POINT('Ctrl Pts',(-0.195647655240959,-0.000106560329145428,
0.43241303078758));
#7603=CARTESIAN_POINT('Ctrl Pts',(-0.195688273475104,-0.00628602257813338,
0.432766621321477));
#7604=CARTESIAN_POINT('Ctrl Pts',(-0.195420885419549,-0.0124619241798928,
0.433120211855374));
#7605=CARTESIAN_POINT('Ctrl Pts',(-0.19483398000204,-0.0186073107818865,
0.433473802389271));
#7606=CARTESIAN_POINT('Ctrl Pts',(-0.188684413786296,-0.0829983705725154,
0.437178706683196));
#7607=CARTESIAN_POINT('Ctrl Pts',(-0.147455848775841,-0.144039266123401,
0.440883610977121));
#7608=CARTESIAN_POINT('Ctrl Pts',(-0.0900196439067171,-0.173790032766202,
0.444588515271047));
#7609=CARTESIAN_POINT('Ctrl Pts',(-0.0325834390375927,-0.203540799409003,
0.448293419564972));
#7610=CARTESIAN_POINT('Ctrl Pts',(0.0410604056902019,-0.202001437143719,
0.451998323858898));
#7611=CARTESIAN_POINT('Ctrl Pts',(0.097203236411656,-0.169876551086573,
0.455703228152823));
#7612=CARTESIAN_POINT('Ctrl Pts',(0.153346067133109,-0.137751665029427,
0.459408132446748));
#7613=CARTESIAN_POINT('Ctrl Pts',(0.191987883848223,-0.0750412551804201,
0.463113036740674));
#7614=CARTESIAN_POINT('Ctrl Pts',(0.195441347863866,-0.0104494652075844,
0.466817941034599));
#7615=CARTESIAN_POINT('Ctrl Pts',(0.19889481187951,0.0541423247652522,0.470522845328524));
#7616=CARTESIAN_POINT('Ctrl Pts',(0.167159923195683,0.120615494861917,0.47422774962245));
#7617=CARTESIAN_POINT('Ctrl Pts',(0.11476254452422,0.158543590700778,0.477932653916375));
#7618=CARTESIAN_POINT('Ctrl Pts',(0.0623651658527581,0.196471686539638,
0.4816375582103));
#7619=CARTESIAN_POINT('Ctrl Pts',(-0.0106947028063393,0.205854708120693,
0.485342462504226));
#7620=CARTESIAN_POINT('Ctrl Pts',(-0.0709757082326437,0.182397808700773,
0.489047366798152));
#7621=CARTESIAN_POINT('Ctrl Pts',(-0.131256713658948,0.158940909280854,
0.492752271092077));
#7622=CARTESIAN_POINT('Ctrl Pts',(-0.17875885585246,0.102644088859959,0.496457175386002));
#7623=CARTESIAN_POINT('Ctrl Pts',(-0.191739200628169,0.0392758287046884,
0.500162079679927));
#7624=CARTESIAN_POINT('Ctrl Pts',(-0.194367979415473,0.026442491766192,
0.500912396715811));
#7625=CARTESIAN_POINT('Ctrl Pts',(-0.195580869792883,0.0133191244610842,
0.501662713751695));
#7626=CARTESIAN_POINT('Ctrl Pts',(-0.19545977166257,0.000173536236839714,
0.502413030787579));
#7627=CARTESIAN_POINT('Origin',(0.,0.,0.));
#7628=CARTESIAN_POINT('',(-0.195080329080103,1.51580434829407E-5,0.582586969212423));
#7629=CARTESIAN_POINT('',(-0.195079254985845,-5.12448512575846E-7,0.57241303078758));
#7630=CARTESIAN_POINT('',(-0.1954,-2.39295984553393E-17,0.));
#7631=CARTESIAN_POINT('Ctrl Pts',(-0.195080329080103,1.51580434829407E-5,
0.582586969212423));
#7632=CARTESIAN_POINT('Ctrl Pts',(-0.195102259420329,0.0317059890063944,
0.580787008604518));
#7633=CARTESIAN_POINT('Ctrl Pts',(-0.187819394734967,0.0633873169979506,
0.578987047996612));
#7634=CARTESIAN_POINT('Ctrl Pts',(-0.173177087283773,0.0911932395442308,
0.577187087388707));
#7635=CARTESIAN_POINT('Ctrl Pts',(-0.14303845674339,0.148426870872502,0.573482183094781));
#7636=CARTESIAN_POINT('Ctrl Pts',(-0.0817200554256732,0.189241561623651,
0.569777278800856));
#7637=CARTESIAN_POINT('Ctrl Pts',(-0.0172888694204259,0.19495539359768,
0.566072374506931));
#7638=CARTESIAN_POINT('Ctrl Pts',(0.0471423165848214,0.200669225571709,
0.562367470213006));
#7639=CARTESIAN_POINT('Ctrl Pts',(0.1146862872776,0.17128219876862,0.55866256591908));
#7640=CARTESIAN_POINT('Ctrl Pts',(0.154426455709376,0.120245500022675,0.554957661625155));
#7641=CARTESIAN_POINT('Ctrl Pts',(0.194166624141151,0.0692088012767304,
0.551252757331229));
#7642=CARTESIAN_POINT('Ctrl Pts',(0.206102990311925,-0.0034775694120695,
0.547547853037304));
#7643=CARTESIAN_POINT('Ctrl Pts',(0.184771976958126,-0.0645432183087307,
0.543842948743378));
#7644=CARTESIAN_POINT('Ctrl Pts',(0.163440963604328,-0.125608867205391,
0.540138044449453));
#7645=CARTESIAN_POINT('Ctrl Pts',(0.10884257072596,-0.175053794309913,0.536433140155528));
#7646=CARTESIAN_POINT('Ctrl Pts',(0.0459678662652951,-0.1902458035534,0.532728235861602));
#7647=CARTESIAN_POINT('Ctrl Pts',(-0.0169068381953713,-0.205437812796887,
0.529023331567677));
#7648=CARTESIAN_POINT('Ctrl Pts',(-0.088057854238333,-0.186376904179337,
0.525318427273751));
#7649=CARTESIAN_POINT('Ctrl Pts',(-0.134917558855844,-0.141787738577927,
0.521613522979826));
#7650=CARTESIAN_POINT('Ctrl Pts',(-0.172973570536371,-0.105575691984742,
0.518604671724025));
#7651=CARTESIAN_POINT('Ctrl Pts',(-0.195008257896402,-0.052526494143854,
0.515595820468224));
#7652=CARTESIAN_POINT('Ctrl Pts',(-0.195488415809582,0.000168817958016994,
0.512586969212423));
#7653=CARTESIAN_POINT('Ctrl Pts',(-0.19545977166257,0.000173536236839714,
0.502413030787579));
#7654=CARTESIAN_POINT('Ctrl Pts',(-0.194982913247146,-0.0515909654461778,
0.505367618045621));
#7655=CARTESIAN_POINT('Ctrl Pts',(-0.173821026745911,-0.103700028070894,
0.508322205303663));
#7656=CARTESIAN_POINT('Ctrl Pts',(-0.136974911436022,-0.139801235384611,
0.511276792561704));
#7657=CARTESIAN_POINT('Ctrl Pts',(-0.0907717301102581,-0.185070339428992,
0.514981696855629));
#7658=CARTESIAN_POINT('Ctrl Pts',(-0.0199068201008233,-0.205168847628107,
0.518686601149554));
#7659=CARTESIAN_POINT('Ctrl Pts',(0.0431831535659995,-0.190897163483548,
0.52239150544348));
#7660=CARTESIAN_POINT('Ctrl Pts',(0.106273127232821,-0.176625479338991,
0.526096409737405));
#7661=CARTESIAN_POINT('Ctrl Pts',(0.161588164557031,-0.127983602850761,
0.529801314031331));
#7662=CARTESIAN_POINT('Ctrl Pts',(0.183809171273742,-0.0672361534713996,
0.533506218325256));
#7663=CARTESIAN_POINT('Ctrl Pts',(0.206030177990453,-0.00648870409203645,
0.537211122619182));
#7664=CARTESIAN_POINT('Ctrl Pts',(0.195157154099664,0.0663643181784591,
0.540916026913107));
#7665=CARTESIAN_POINT('Ctrl Pts',(0.156166958158329,0.117976238953206,0.544620931207032));
#7666=CARTESIAN_POINT('Ctrl Pts',(0.117176762216995,0.169588159727953,0.548325835500957));
#7667=CARTESIAN_POINT('Ctrl Pts',(0.0500693942251149,0.19995897900695,0.552030739794883));
#7668=CARTESIAN_POINT('Ctrl Pts',(-0.014438402988479,0.195187203210435,
0.555735644088809));
#7669=CARTESIAN_POINT('Ctrl Pts',(-0.0789462002020729,0.19041542741392,
0.559440548382734));
#7670=CARTESIAN_POINT('Ctrl Pts',(-0.140854426637381,0.150501056541893,
0.563145452676659));
#7671=CARTESIAN_POINT('Ctrl Pts',(-0.171826118302126,0.0937139095715946,
0.566850356970585));
#7672=CARTESIAN_POINT('Ctrl Pts',(-0.18732678126338,0.0652931686173718,
0.56870458157625));
#7673=CARTESIAN_POINT('Ctrl Pts',(-0.19507850314188,0.0326461576927833,
0.570558806181915));
#7674=CARTESIAN_POINT('Ctrl Pts',(-0.195079266632945,-5.12429904213991E-7,
0.57241303078758));
#7675=CARTESIAN_POINT('Origin',(0.,0.,0.));
#7676=CARTESIAN_POINT('',(-0.195432764861167,-0.000176589099362662,0.652586969212424));
#7677=CARTESIAN_POINT('',(-0.195461653185843,-0.000173273723800459,0.64241303078758));
#7678=CARTESIAN_POINT('',(-0.1954,-2.39295984553393E-17,0.));
#7679=CARTESIAN_POINT('Ctrl Pts',(-0.195432764861167,-0.000176589099362662,
0.652586969212424));
#7680=CARTESIAN_POINT('Ctrl Pts',(-0.19496258822817,0.050717369554878,0.649683101034737));
#7681=CARTESIAN_POINT('Ctrl Pts',(-0.174597076629887,0.101944751897959,
0.646779232857051));
#7682=CARTESIAN_POINT('Ctrl Pts',(-0.138871424621133,0.137917504046295,
0.643875364679364));
#7683=CARTESIAN_POINT('Ctrl Pts',(-0.0932908013175052,0.183813390410141,
0.640170460385439));
#7684=CARTESIAN_POINT('Ctrl Pts',(-0.0227069904956954,0.204877838448089,
0.636465556091513));
#7685=CARTESIAN_POINT('Ctrl Pts',(0.040572009039235,0.19146911652061,0.632760651797588));
#7686=CARTESIAN_POINT('Ctrl Pts',(0.103851008574166,0.178060394593131,0.629055747503662));
#7687=CARTESIAN_POINT('Ctrl Pts',(0.159825196822218,0.130178502700225,0.625350843209737));
#7688=CARTESIAN_POINT('Ctrl Pts',(0.182873769437794,0.0697401960871604,
0.621645938915812));
#7689=CARTESIAN_POINT('Ctrl Pts',(0.205922342053369,0.00930188947409603,
0.617941034621886));
#7690=CARTESIAN_POINT('Ctrl Pts',(0.196045299036468,-0.0636928318591254,
0.614236130327961));
#7691=CARTESIAN_POINT('Ctrl Pts',(0.157763613259938,-0.115832434273962,
0.610531226034036));
#7692=CARTESIAN_POINT('Ctrl Pts',(0.119481927483407,-0.167972036688798,
0.60682632174011));
#7693=CARTESIAN_POINT('Ctrl Pts',(0.0527955989472468,-0.199256520185249,
0.603121417446185));
#7694=CARTESIAN_POINT('Ctrl Pts',(-0.0117713499477233,-0.195366183918996,
0.599416513152259));
#7695=CARTESIAN_POINT('Ctrl Pts',(-0.0763382988426937,-0.191475847652744,
0.595711608858334));
#7696=CARTESIAN_POINT('Ctrl Pts',(-0.138785868096474,-0.152410691623788,
0.592006704564409));
#7697=CARTESIAN_POINT('Ctrl Pts',(-0.170530222841839,-0.0960518276566117,
0.588301800270483));
#7698=CARTESIAN_POINT('Ctrl Pts',(-0.186852158131264,-0.0670738963665755,
0.586396856584463));
#7699=CARTESIAN_POINT('Ctrl Pts',(-0.195057119648206,-0.0335240472493347,
0.584491912898443));
#7700=CARTESIAN_POINT('Ctrl Pts',(-0.195080329080103,1.51580434829407E-5,
0.582586969212423));
#7701=CARTESIAN_POINT('Ctrl Pts',(-0.195079266632945,-5.12429904213991E-7,
0.57241303078758));
#7702=CARTESIAN_POINT('Ctrl Pts',(-0.195080028664364,-0.0325847684584389,
0.57426371047584));
#7703=CARTESIAN_POINT('Ctrl Pts',(-0.187359440633393,-0.0651686849869207,
0.5761143901641));
#7704=CARTESIAN_POINT('Ctrl Pts',(-0.17191549678333,-0.0935498463051126,
0.577965069852361));
#7705=CARTESIAN_POINT('Ctrl Pts',(-0.140998026705607,-0.150366532142949,
0.581669974146286));
#7706=CARTESIAN_POINT('Ctrl Pts',(-0.0791279296559783,-0.190339980750052,
0.585374878440212));
#7707=CARTESIAN_POINT('Ctrl Pts',(-0.0146247168406994,-0.195173331772808,
0.589079782734137));
#7708=CARTESIAN_POINT('Ctrl Pts',(0.0498784959745796,-0.200006682795564,
0.592784687028062));
#7709=CARTESIAN_POINT('Ctrl Pts',(0.11701482455551,-0.169699936233974,0.596489591321988));
#7710=CARTESIAN_POINT('Ctrl Pts',(0.156054270077791,-0.118125257961442,
0.600194495615913));
#7711=CARTESIAN_POINT('Ctrl Pts',(0.195093715600072,-0.0665505796889094,
0.603899399909839));
#7712=CARTESIAN_POINT('Ctrl Pts',(0.206036278063704,0.00629203029456468,
0.607604304203764));
#7713=CARTESIAN_POINT('Ctrl Pts',(0.183873269344836,0.0670606635697158,
0.611309208497689));
#7714=CARTESIAN_POINT('Ctrl Pts',(0.161710260625969,0.127829296844866,0.615014112791615));
#7715=CARTESIAN_POINT('Ctrl Pts',(0.106441680724601,0.176523953411694,0.61871901708554));
#7716=CARTESIAN_POINT('Ctrl Pts',(0.0433653591659573,0.190855855038238,
0.622423921379465));
#7717=CARTESIAN_POINT('Ctrl Pts',(-0.0197109623926868,0.205187756664782,
0.626128825673391));
#7718=CARTESIAN_POINT('Ctrl Pts',(-0.0905950256086064,0.185156903351043,
0.629833729967317));
#7719=CARTESIAN_POINT('Ctrl Pts',(-0.136841398547571,0.139931924240018,
0.633538634261242));
#7720=CARTESIAN_POINT('Ctrl Pts',(-0.173766207647965,0.103822633627155,
0.636496766436688));
#7721=CARTESIAN_POINT('Ctrl Pts',(-0.194984453966749,0.0516520517928096,
0.639454898612134));
#7722=CARTESIAN_POINT('Ctrl Pts',(-0.195461653185843,-0.000173273723800459,
0.64241303078758));
#7723=CARTESIAN_POINT('Origin',(0.,0.,0.));
#7724=CARTESIAN_POINT('',(-0.195665606136028,9.31787759667347E-5,0.722586969212424));
#7725=CARTESIAN_POINT('',(-0.195646327283704,0.000107461668706292,0.712413030787581));
#7726=CARTESIAN_POINT('',(-0.1954,-2.39295984553393E-17,0.));
#7727=CARTESIAN_POINT('Ctrl Pts',(-0.195665606136028,9.31787759667347E-5,
0.722586969212424));
#7728=CARTESIAN_POINT('Ctrl Pts',(-0.195696782701144,0.0053849756768864,
0.722284097758882));
#7729=CARTESIAN_POINT('Ctrl Pts',(-0.1955007119948,0.0106744267763307,0.72198122630534));
#7730=CARTESIAN_POINT('Ctrl Pts',(-0.19506992917185,0.0159446928961413,
0.721678354851798));
#7731=CARTESIAN_POINT('Ctrl Pts',(-0.189800336703391,0.0804137319853543,
0.717973450557872));
#7732=CARTESIAN_POINT('Ctrl Pts',(-0.149409263832838,0.142011999441816,
0.714268546263947));
#7733=CARTESIAN_POINT('Ctrl Pts',(-0.0923847281217706,0.172544407352221,
0.710563641970021));
#7734=CARTESIAN_POINT('Ctrl Pts',(-0.0353601924107021,0.203076815262627,
0.706858737676096));
#7735=CARTESIAN_POINT('Ctrl Pts',(0.0382978061408807,0.202543363626974,
0.70315383338217));
#7736=CARTESIAN_POINT('Ctrl Pts',(0.0948741351041633,0.171188226776551,
0.699448929088245));
#7737=CARTESIAN_POINT('Ctrl Pts',(0.151450464067444,0.139833089926128,0.695744024794319));
#7738=CARTESIAN_POINT('Ctrl Pts',(0.190945123442426,0.0776562678609379,
0.692039120500394));
#7739=CARTESIAN_POINT('Ctrl Pts',(0.195280406839545,0.0131176675992589,
0.688334216206469));
#7740=CARTESIAN_POINT('Ctrl Pts',(0.199615690236664,-0.0514209326624214,
0.684629311912544));
#7741=CARTESIAN_POINT('Ctrl Pts',(0.168791597655919,-0.118321311120591,
0.680924407618618));
#7742=CARTESIAN_POINT('Ctrl Pts',(0.116917097353215,-0.156961469301105,
0.677219503324692));
#7743=CARTESIAN_POINT('Ctrl Pts',(0.0650425970505132,-0.195601627481618,
0.673514599030767));
#7744=CARTESIAN_POINT('Ctrl Pts',(-0.0078823109741457,-0.205981565384478,
0.669809694736841));
#7745=CARTESIAN_POINT('Ctrl Pts',(-0.0684780484026163,-0.183350122404191,
0.666104790442916));
#7746=CARTESIAN_POINT('Ctrl Pts',(-0.129073785831088,-0.160718679423904,
0.662399886148991));
#7747=CARTESIAN_POINT('Ctrl Pts',(-0.17734035266337,-0.105075855560469,
0.658694981855066));
#7748=CARTESIAN_POINT('Ctrl Pts',(-0.191184918186788,-0.0418907812838809,
0.65499007756114));
#7749=CARTESIAN_POINT('Ctrl Pts',(-0.194178247060648,-0.0282295575416714,
0.654189041444902));
#7750=CARTESIAN_POINT('Ctrl Pts',(-0.195562463745895,-0.0142157590911969,
0.653388005328663));
#7751=CARTESIAN_POINT('Ctrl Pts',(-0.195432764861167,-0.000176589099362662,
0.652586969212424));
#7752=CARTESIAN_POINT('Ctrl Pts',(-0.195461653185843,-0.000173273723800459,
0.64241303078758));
#7753=CARTESIAN_POINT('Ctrl Pts',(-0.195582120781827,-0.0132564308755209,
0.643159802906059));
#7754=CARTESIAN_POINT('Ctrl Pts',(-0.194380770210329,-0.026317584988001,
0.643906575024539));
#7755=CARTESIAN_POINT('Ctrl Pts',(-0.19177660491574,-0.0390927817501061,
0.644653347143018));
#7756=CARTESIAN_POINT('Ctrl Pts',(-0.178856755682938,-0.102473403720895,
0.648358251436943));
#7757=CARTESIAN_POINT('Ctrl Pts',(-0.131408374555326,-0.158815542754161,
0.652063155730869));
#7758=CARTESIAN_POINT('Ctrl Pts',(-0.0711497879157472,-0.182329974106052,
0.655768060024794));
#7759=CARTESIAN_POINT('Ctrl Pts',(-0.0108912012761686,-0.205844405457942,
0.65947296431872));
#7760=CARTESIAN_POINT('Ctrl Pts',(0.0621775908753766,-0.196531129128456,
0.663177868612645));
#7761=CARTESIAN_POINT('Ctrl Pts',(0.114611150809846,-0.158653067691778,
0.66688277290657));
#7762=CARTESIAN_POINT('Ctrl Pts',(0.167044710744316,-0.1207750062551,0.670587677200496));
#7763=CARTESIAN_POINT('Ctrl Pts',(0.19884303846171,-0.0543321597112302,
0.674292581494421));
#7764=CARTESIAN_POINT('Ctrl Pts',(0.195451233596986,0.0102628974167111,
0.677997485788347));
#7765=CARTESIAN_POINT('Ctrl Pts',(0.192059428732261,0.0748579545446525,
0.681702390082272));
#7766=CARTESIAN_POINT('Ctrl Pts',(0.153477491285418,0.137605222256665,0.685407294376197));
#7767=CARTESIAN_POINT('Ctrl Pts',(0.0973653516911611,0.16978368610684,0.689112198670123));
#7768=CARTESIAN_POINT('Ctrl Pts',(0.0412532120969042,0.201962149957014,
0.692817102964048));
#7769=CARTESIAN_POINT('Ctrl Pts',(-0.0323891296447666,0.203571809945351,
0.696522007257973));
#7770=CARTESIAN_POINT('Ctrl Pts',(-0.089853707623677,0.173875883906447,
0.700226911551899));
#7771=CARTESIAN_POINT('Ctrl Pts',(-0.147318285602587,0.144179957867542,
0.703931815845824));
#7772=CARTESIAN_POINT('Ctrl Pts',(-0.188605099818737,0.0831784458013958,
0.70763672013975));
#7773=CARTESIAN_POINT('Ctrl Pts',(-0.194816129198604,0.0187932855574017,
0.711341624433676));
#7774=CARTESIAN_POINT('Ctrl Pts',(-0.195414843390564,0.0125868571488267,
0.711698759884977));
#7775=CARTESIAN_POINT('Ctrl Pts',(-0.195687631335538,0.00634898768321266,
0.712055895336279));
#7776=CARTESIAN_POINT('Ctrl Pts',(-0.195646327283704,0.000107461668706292,
0.712413030787581));
#7777=CARTESIAN_POINT('Origin',(0.,0.,0.));
#7778=CARTESIAN_POINT('',(-0.195153751526609,0.000118248258768078,0.792586969212424));
#7779=CARTESIAN_POINT('',(-0.195137151677628,0.000105948740446043,0.78241303078758));
#7780=CARTESIAN_POINT('',(-0.1954,-2.39295984553393E-17,0.));
#7781=CARTESIAN_POINT('Ctrl Pts',(-0.195153751526609,0.000118248258768078,
0.792586969212424));
#7782=CARTESIAN_POINT('Ctrl Pts',(-0.195290424219172,0.0248632703434088,
0.7911801901891));
#7783=CARTESIAN_POINT('Ctrl Pts',(-0.190927662847405,0.0495618887102773,
0.789773411165777));
#7784=CARTESIAN_POINT('Ctrl Pts',(-0.181844484105553,0.0723815867403318,
0.788366632142454));
#7785=CARTESIAN_POINT('Ctrl Pts',(-0.157922953171942,0.132479722848387,
0.784661727848529));
#7786=CARTESIAN_POINT('Ctrl Pts',(-0.101261124890318,0.179545873498893,
0.780956823554603));
#7787=CARTESIAN_POINT('Ctrl Pts',(-0.0377945538744258,0.192036668884086,
0.777251919260678));
#7788=CARTESIAN_POINT('Ctrl Pts',(0.0256720171414684,0.204527464269279,
0.773547014966752));
#7789=CARTESIAN_POINT('Ctrl Pts',(0.0959433308916326,0.182442904389159,
0.769842110672827));
#7790=CARTESIAN_POINT('Ctrl Pts',(0.140854426399365,0.135891651923026,0.766137206378902));
#7791=CARTESIAN_POINT('Ctrl Pts',(0.185765521907095,0.0893403994568938,
0.762432302084977));
#7792=CARTESIAN_POINT('Ctrl Pts',(0.205316399172396,0.0183224544047523,
0.758727397791051));
#7793=CARTESIAN_POINT('Ctrl Pts',(0.190558126252222,-0.04465547019017,0.755022493497126));
#7794=CARTESIAN_POINT('Ctrl Pts',(0.175799853332047,-0.107633394785094,
0.7513175892032));
#7795=CARTESIAN_POINT('Ctrl Pts',(0.126732430226394,-0.162571298922797,
0.747612684909275));
#7796=CARTESIAN_POINT('Ctrl Pts',(0.065815259857937,-0.184322711754398,
0.74390778061535));
#7797=CARTESIAN_POINT('Ctrl Pts',(0.00489808948948139,-0.206074124586,0.740202876321424));
#7798=CARTESIAN_POINT('Ctrl Pts',(-0.0678688281417779,-0.194639046111501,
0.736497972027499));
#7799=CARTESIAN_POINT('Ctrl Pts',(-0.119178230924225,-0.155251601513269,
0.732793067733573));
#7800=CARTESIAN_POINT('Ctrl Pts',(-0.166293151968891,-0.119084032963209,
0.72939103489319));
#7801=CARTESIAN_POINT('Ctrl Pts',(-0.195315412358655,-0.0593474407707721,
0.725989002052807));
#7802=CARTESIAN_POINT('Ctrl Pts',(-0.195665606136028,9.31787759667347E-5,
0.722586969212424));
#7803=CARTESIAN_POINT('Ctrl Pts',(-0.195646327283704,0.000107461668706292,
0.712413030787581));
#7804=CARTESIAN_POINT('Ctrl Pts',(-0.19525914528511,-0.0584002732694843,
0.715760799630204));
#7805=CARTESIAN_POINT('Ctrl Pts',(-0.167272421555789,-0.117229312394887,
0.719108568472827));
#7806=CARTESIAN_POINT('Ctrl Pts',(-0.121433992833904,-0.153493638833617,
0.722456337315451));
#7807=CARTESIAN_POINT('Ctrl Pts',(-0.0707055825457531,-0.193626594558799,
0.726161241609376));
#7808=CARTESIAN_POINT('Ctrl Pts',(0.00188648257413163,-0.206123697587321,
0.729866145903302));
#7809=CARTESIAN_POINT('Ctrl Pts',(0.0631149748393498,-0.185264707186764,
0.733571050197227));
#7810=CARTESIAN_POINT('Ctrl Pts',(0.124343467104567,-0.164405716786208,
0.737275954491153));
#7811=CARTESIAN_POINT('Ctrl Pts',(0.174208386515118,-0.110190632956576,
0.740980858785078));
#7812=CARTESIAN_POINT('Ctrl Pts',(0.189885295881042,-0.0474350733754927,
0.744685763079003));
#7813=CARTESIAN_POINT('Ctrl Pts',(0.205562205246967,0.0153204862055921,
0.748390667372929));
#7814=CARTESIAN_POINT('Ctrl Pts',(0.187051104568262,0.0866165215381275,
0.752095571666854));
#7815=CARTESIAN_POINT('Ctrl Pts',(0.142824993696378,0.133819030610743,0.75580047596078));
#7816=CARTESIAN_POINT('Ctrl Pts',(0.0985988828244949,0.181021539683357,
0.759505380254705));
#7817=CARTESIAN_POINT('Ctrl Pts',(0.0286577617594329,0.204130522496052,
0.76321028454863));
#7818=CARTESIAN_POINT('Ctrl Pts',(-0.0349845460811521,0.192568412034438,
0.766915188842556));
#7819=CARTESIAN_POINT('Ctrl Pts',(-0.0986268539217371,0.181006301572824,
0.770620093136481));
#7820=CARTESIAN_POINT('Ctrl Pts',(-0.155970348537846,0.1347730978369,0.774324997430407));
#7821=CARTESIAN_POINT('Ctrl Pts',(-0.180767459361033,0.0750309097247715,
0.778029901724332));
#7822=CARTESIAN_POINT('Ctrl Pts',(-0.190546293802352,0.0514713518844925,
0.779490944745415));
#7823=CARTESIAN_POINT('Ctrl Pts',(-0.195263680442012,0.025810945614826,
0.780951987766498));
#7824=CARTESIAN_POINT('Ctrl Pts',(-0.195137151677628,0.000105948740446043,
0.78241303078758));
#7825=CARTESIAN_POINT('Origin',(0.,0.,0.));
#7826=CARTESIAN_POINT('',(-0.195235475305001,-0.000156905063299573,0.862586969212423));
#7827=CARTESIAN_POINT('',(-0.195259979386646,-0.000163936101596873,0.85241303078758));
#7828=CARTESIAN_POINT('',(-0.1954,-2.39295984553393E-17,0.));
#7829=CARTESIAN_POINT('Ctrl Pts',(-0.195235475305001,-0.000156905063299573,
0.862586969212423));
#7830=CARTESIAN_POINT('Ctrl Pts',(-0.194902940139162,0.0439592076248328,
0.860076282619319));
#7831=CARTESIAN_POINT('Ctrl Pts',(-0.18009730434855,0.0882774316754031,
0.857565596026215));
#7832=CARTESIAN_POINT('Ctrl Pts',(-0.152668645933159,0.122469567842785,
0.855054909433111));
#7833=CARTESIAN_POINT('Ctrl Pts',(-0.112193441015542,0.172925324627786,
0.851350005139186));
#7834=CARTESIAN_POINT('Ctrl Pts',(-0.0442309197344043,0.201330975868051,
0.84764510084526));
#7835=CARTESIAN_POINT('Ctrl Pts',(0.0201107497513655,0.194684535192451,
0.843940196551335));
#7836=CARTESIAN_POINT('Ctrl Pts',(0.0844524192371344,0.188038094516851,
0.84023529225741));
#7837=CARTESIAN_POINT('Ctrl Pts',(0.145173236927535,0.14633956192539,0.836530387963485));
#7838=CARTESIAN_POINT('Ctrl Pts',(0.174479745901743,0.0886754124248997,
0.832825483669559));
#7839=CARTESIAN_POINT('Ctrl Pts',(0.203786254875951,0.0310112629244105,
0.829120579375634));
#7840=CARTESIAN_POINT('Ctrl Pts',(0.201678455133965,-0.0426185034851084,
0.825415675081708));
#7841=CARTESIAN_POINT('Ctrl Pts',(0.169121140029283,-0.0985116769416633,
0.821710770787783));
#7842=CARTESIAN_POINT('Ctrl Pts',(0.136563824924599,-0.15440485039822,0.818005866493857));
#7843=CARTESIAN_POINT('Ctrl Pts',(0.0735569944572206,-0.192561430901813,
0.814300962199932));
#7844=CARTESIAN_POINT('Ctrl Pts',(0.00894047152349694,-0.195516184669199,
0.810596057906007));
#7845=CARTESIAN_POINT('Ctrl Pts',(-0.0556760514102258,-0.198470938436586,
0.806891153612081));
#7846=CARTESIAN_POINT('Ctrl Pts',(-0.121902266810292,-0.166223865467764,
0.803186249318156));
#7847=CARTESIAN_POINT('Ctrl Pts',(-0.159424757717526,-0.11353526820055,
0.799481345024231));
#7848=CARTESIAN_POINT('Ctrl Pts',(-0.182699686765289,-0.0808529133416383,
0.797183219753628));
#7849=CARTESIAN_POINT('Ctrl Pts',(-0.194930481941712,-0.0403054143289745,
0.794885094483026));
#7850=CARTESIAN_POINT('Ctrl Pts',(-0.195153751526609,0.000118248258768078,
0.792586969212424));
#7851=CARTESIAN_POINT('Ctrl Pts',(-0.195137151677628,0.000105948740446043,
0.78241303078758));
#7852=CARTESIAN_POINT('Ctrl Pts',(-0.194942829545969,-0.0393716341730415,
0.784656892060423));
#7853=CARTESIAN_POINT('Ctrl Pts',(-0.183323340652406,-0.0789543913210836,
0.786900753333265));
#7854=CARTESIAN_POINT('Ctrl Pts',(-0.161066679056451,-0.111193689909524,
0.789144614606108));
#7855=CARTESIAN_POINT('Ctrl Pts',(-0.124318060898417,-0.164424928943361,
0.792849518900033));
#7856=CARTESIAN_POINT('Ctrl Pts',(-0.0585700975520817,-0.197636234522699,
0.796554423193959));
#7857=CARTESIAN_POINT('Ctrl Pts',(0.00608270210726663,-0.195625950510262,
0.800259327487884));
#7858=CARTESIAN_POINT('Ctrl Pts',(0.070735501766615,-0.193615666497825,
0.80396423178181));
#7859=CARTESIAN_POINT('Ctrl Pts',(0.134293137738976,-0.156383792893612,
0.807669136075735));
#7860=CARTESIAN_POINT('Ctrl Pts',(0.167663669490968,-0.100972301700975,
0.811374040369661));
#7861=CARTESIAN_POINT('Ctrl Pts',(0.20103420124296,-0.0455608105083384,
0.815078944663586));
#7862=CARTESIAN_POINT('Ctrl Pts',(0.204217628774584,0.0280302982727214,
0.818783848957511));
#7863=CARTESIAN_POINT('Ctrl Pts',(0.175756816636647,0.0861165093563451,
0.822488753251437));
#7864=CARTESIAN_POINT('Ctrl Pts',(0.147296004498709,0.14420272043997,0.826193657545363));
#7865=CARTESIAN_POINT('Ctrl Pts',(0.0871909526912083,0.186784033826158,
0.829898561839288));
#7866=CARTESIAN_POINT('Ctrl Pts',(0.022953266486877,0.194369903368684,0.833603466133213));
#7867=CARTESIAN_POINT('Ctrl Pts',(-0.0412844197174542,0.201955772911211,
0.837308370427139));
#7868=CARTESIAN_POINT('Ctrl Pts',(-0.109654740318616,0.174546198610077,
0.841013274721063));
#7869=CARTESIAN_POINT('Ctrl Pts',(-0.150862867075323,0.124687237180806,
0.844718179014989));
#7870=CARTESIAN_POINT('Ctrl Pts',(-0.179391757618137,0.0901692679076088,
0.847283129605853));
#7871=CARTESIAN_POINT('Ctrl Pts',(-0.194901910843352,0.0448913918449987,
0.849848080196716));
#7872=CARTESIAN_POINT('Ctrl Pts',(-0.195259979386646,-0.000163936101596873,
0.85241303078758));
#7873=CARTESIAN_POINT('Origin',(0.,0.,0.));
#7874=CARTESIAN_POINT('',(-0.195715067010162,-2.931307771456E-5,0.932586969212424));
#7875=CARTESIAN_POINT('',(-0.195719607651052,-1.17545938899131E-5,0.922413030787581));
#7876=CARTESIAN_POINT('',(-0.1954,-2.39295984553393E-17,0.));
#7877=CARTESIAN_POINT('Ctrl Pts',(-0.195715067010162,-2.931307771456E-5,
0.932586969212424));
#7878=CARTESIAN_POINT('Ctrl Pts',(-0.195582961786627,0.0630827139603783,
0.928972375049538));
#7879=CARTESIAN_POINT('Ctrl Pts',(-0.162276589664832,0.126314497964337,
0.925357780886653));
#7880=CARTESIAN_POINT('Ctrl Pts',(-0.110101557926667,0.161815195333392,
0.921743186723768));
#7881=CARTESIAN_POINT('Ctrl Pts',(-0.0566229402972577,0.19820287267501,
0.918038282429843));
#7882=CARTESIAN_POINT('Ctrl Pts',(0.0166789772399235,0.205456437773955,
0.914333378135918));
#7883=CARTESIAN_POINT('Ctrl Pts',(0.076252049559439,0.180255750079291,0.910628473841992));
#7884=CARTESIAN_POINT('Ctrl Pts',(0.135825121878954,0.155055062384626,0.906923569548067));
#7885=CARTESIAN_POINT('Ctrl Pts',(0.181669348980803,0.0974001218963517,
0.903218665254141));
#7886=CARTESIAN_POINT('Ctrl Pts',(0.192800666428956,0.0336810558506326,
0.899513760960216));
#7887=CARTESIAN_POINT('Ctrl Pts',(0.203931983877108,-0.0300380101950847,
0.895808856666291));
#7888=CARTESIAN_POINT('Ctrl Pts',(0.180350391671563,-0.0998212017982479,
0.892103952372366));
#7889=CARTESIAN_POINT('Ctrl Pts',(0.13284978212173,-0.143726983857839,0.88839904807844));
#7890=CARTESIAN_POINT('Ctrl Pts',(0.0853491725718961,-0.187632765917432,
0.884694143784515));
#7891=CARTESIAN_POINT('Ctrl Pts',(0.013929545677772,-0.205661138433453,
0.880989239490589));
#7892=CARTESIAN_POINT('Ctrl Pts',(-0.048718525559727,-0.189560058466833,
0.877284335196664));
#7893=CARTESIAN_POINT('Ctrl Pts',(-0.111366596797226,-0.173458978500212,
0.873579430902738));
#7894=CARTESIAN_POINT('Ctrl Pts',(-0.165243112378099,-0.123228446050951,
0.869874526608813));
#7895=CARTESIAN_POINT('Ctrl Pts',(-0.185687425891486,-0.0618602486614515,
0.866169622314888));
#7896=CARTESIAN_POINT('Ctrl Pts',(-0.192277329203931,-0.0420791742325638,
0.864975404614066));
#7897=CARTESIAN_POINT('Ctrl Pts',(-0.195393646931154,-0.0211409031490452,
0.863781186913245));
#7898=CARTESIAN_POINT('Ctrl Pts',(-0.195235475305001,-0.000156905063299573,
0.862586969212423));
#7899=CARTESIAN_POINT('Ctrl Pts',(-0.195259979386646,-0.000163936101596873,
0.85241303078758));
#7900=CARTESIAN_POINT('Ctrl Pts',(-0.19541911756394,-0.0201880987963234,
0.853552984490642));
#7901=CARTESIAN_POINT('Ctrl Pts',(-0.192585379153193,-0.0401683032463519,
0.854692938193704));
#7902=CARTESIAN_POINT('Ctrl Pts',(-0.186571486394569,-0.0591404450650352,
0.855832891896766));
#7903=CARTESIAN_POINT('Ctrl Pts',(-0.167026046044856,-0.120800817324193,
0.859537796190691));
#7904=CARTESIAN_POINT('Ctrl Pts',(-0.11388923243318,-0.171813213285104,
0.863242700484616));
#7905=CARTESIAN_POINT('Ctrl Pts',(-0.0514831116350698,-0.188827966663681,
0.866947604778541));
#7906=CARTESIAN_POINT('Ctrl Pts',(0.0109230091630432,-0.205842720042259,
0.870652509072467));
#7907=CARTESIAN_POINT('Ctrl Pts',(0.0825984371475908,-0.188859830838501,
0.874357413366393));
#7908=CARTESIAN_POINT('Ctrl Pts',(0.130735512676577,-0.145652797786935,
0.878062317660318));
#7909=CARTESIAN_POINT('Ctrl Pts',(0.178872588205563,-0.10244576473537,0.881767221954244));
#7910=CARTESIAN_POINT('Ctrl Pts',(0.203471311278988,-0.0330145878359957,
0.885472126248168));
#7911=CARTESIAN_POINT('Ctrl Pts',(0.193272223015147,0.0308603238601364,
0.889177030542094));
#7912=CARTESIAN_POINT('Ctrl Pts',(0.183073134751306,0.0947352355562703,
0.892881934836019));
#7913=CARTESIAN_POINT('Ctrl Pts',(0.138076235150198,0.153053882049163,0.896586839129945));
#7914=CARTESIAN_POINT('Ctrl Pts',(0.0788777453795076,0.179122341046043,
0.900291743423871));
#7915=CARTESIAN_POINT('Ctrl Pts',(0.0196792556088182,0.205190800042922,
0.903996647717796));
#7916=CARTESIAN_POINT('Ctrl Pts',(-0.0537208243314517,0.199009071543789,
0.907701552011721));
#7917=CARTESIAN_POINT('Ctrl Pts',(-0.107725417896538,0.163406689327535,
0.911406456305646));
#7918=CARTESIAN_POINT('Ctrl Pts',(-0.161204584453802,0.128150693444819,
0.915075314466291));
#7919=CARTESIAN_POINT('Ctrl Pts',(-0.195663837766578,0.0640437437643291,
0.918744172626936));
#7920=CARTESIAN_POINT('Ctrl Pts',(-0.195719607651052,-1.17545938899131E-5,
0.922413030787581));
#7921=CARTESIAN_POINT('Origin',(0.,0.,0.));
#7922=CARTESIAN_POINT('',(-0.195321337055717,0.000175186119862003,1.00258696921242));
#7923=CARTESIAN_POINT('',(-0.195294337528581,0.000171262189333537,0.99241303078758));
#7924=CARTESIAN_POINT('',(-0.1954,-2.39295984553393E-17,0.));
#7925=CARTESIAN_POINT('Ctrl Pts',(-0.195321337055717,0.000175186119862003,
1.00258696921242));
#7926=CARTESIAN_POINT('Ctrl Pts',(-0.195476146868043,0.0179656372844682,
1.00157337177368));
#7927=CARTESIAN_POINT('Ctrl Pts',(-0.193245700725841,0.0357179689540282,
1.00055977433494));
#7928=CARTESIAN_POINT('Ctrl Pts',(-0.188475369241895,0.0527593184925091,
0.999546176896202));
#7929=CARTESIAN_POINT('Ctrl Pts',(-0.171038839784721,0.115048908685087,
0.995841272602277));
#7930=CARTESIAN_POINT('Ctrl Pts',(-0.119668151355893,0.167839416275189,
0.992136368308351));
#7931=CARTESIAN_POINT('Ctrl Pts',(-0.0578769697811842,0.186967288228745,
0.988431464014425));
#7932=CARTESIAN_POINT('Ctrl Pts',(0.00391421179352416,0.206095160182302,
0.9847265597205));
#7933=CARTESIAN_POINT('Ctrl Pts',(0.0761258865141124,0.191560396499312,
0.981021655426575));
#7934=CARTESIAN_POINT('Ctrl Pts',(0.125704941019021,0.150015926828012,0.977316751132649));
#7935=CARTESIAN_POINT('Ctrl Pts',(0.175283995523929,0.108471457156712,0.973611846838724));
#7936=CARTESIAN_POINT('Ctrl Pts',(0.202230429813157,0.0399172814971016,
0.969906942544799));
#7937=CARTESIAN_POINT('Ctrl Pts',(0.194210178090586,-0.0242676167903992,
0.966202038250873));
#7938=CARTESIAN_POINT('Ctrl Pts',(0.186189926368015,-0.0884525150779,0.962497133956948));
#7939=CARTESIAN_POINT('Ctrl Pts',(0.143202988633645,-0.148268135993291,
0.958792229663022));
#7940=CARTESIAN_POINT('Ctrl Pts',(0.084925575576374,-0.176335354117331,
0.955087325369097));
#7941=CARTESIAN_POINT('Ctrl Pts',(0.0266481625191027,-0.20440257224137,
0.951382421075171));
#7942=CARTESIAN_POINT('Ctrl Pts',(-0.0469197258610698,-0.200721387574058,
0.947677516781246));
#7943=CARTESIAN_POINT('Ctrl Pts',(-0.102104202844174,-0.166976771618745,
0.943972612487321));
#7944=CARTESIAN_POINT('Ctrl Pts',(-0.157288679827278,-0.133232155663433,
0.940267708193395));
#7945=CARTESIAN_POINT('Ctrl Pts',(-0.194089745413313,-0.0694241084201192,
0.93656280389947));
#7946=CARTESIAN_POINT('Ctrl Pts',(-0.195662619345512,-0.00475919000631662,
0.932857899605544));
#7947=CARTESIAN_POINT('Ctrl Pts',(-0.195700959458955,-0.00318292870714216,
0.932767589474504));
#7948=CARTESIAN_POINT('Ctrl Pts',(-0.195718367640748,-0.0016061582711675,
0.932677279343464));
#7949=CARTESIAN_POINT('Ctrl Pts',(-0.195715067010162,-2.931307771456E-5,
0.932586969212424));
#7950=CARTESIAN_POINT('Ctrl Pts',(-0.195719607651052,-1.17545938899131E-5,
0.922413030787581));
#7951=CARTESIAN_POINT('Ctrl Pts',(-0.195720155584114,-0.000641092913902824,
0.922449076920861));
#7952=CARTESIAN_POINT('Ctrl Pts',(-0.195717382600782,-0.00127042626739718,
0.922485123054142));
#7953=CARTESIAN_POINT('Ctrl Pts',(-0.195711274111555,-0.00189972724385319,
0.922521169187423));
#7954=CARTESIAN_POINT('Ctrl Pts',(-0.195083429571586,-0.0665807256656151,
0.926226073481348));
#7955=CARTESIAN_POINT('Ctrl Pts',(-0.159218633301743,-0.130919686575766,
0.929930977775273));
#7956=CARTESIAN_POINT('Ctrl Pts',(-0.104533111367734,-0.165467037218143,
0.933635882069199));
#7957=CARTESIAN_POINT('Ctrl Pts',(-0.0498475894337254,-0.20001438786052,
0.937340786363124));
#7958=CARTESIAN_POINT('Ctrl Pts',(0.0236586581644487,-0.204770128235125,
0.94104569065705));
#7959=CARTESIAN_POINT('Ctrl Pts',(0.0823399592547179,-0.177557435462165,
0.944750594950975));
#7960=CARTESIAN_POINT('Ctrl Pts',(0.141021260344988,-0.150344742689204,
0.9484554992449));
#7961=CARTESIAN_POINT('Ctrl Pts',(0.184877614927351,-0.091163616768676,
0.952160403538825));
#7962=CARTESIAN_POINT('Ctrl Pts',(0.193834858190581,-0.0271027586825891,
0.955865307832751));
#7963=CARTESIAN_POINT('Ctrl Pts',(0.202792101453811,0.0369580994034978,
0.959570212126676));
#7964=CARTESIAN_POINT('Ctrl Pts',(0.17685023339791,0.105898689655145,0.963275116420602));
#7965=CARTESIAN_POINT('Ctrl Pts',(0.12788350439832,0.14816315696142,0.966980020714527));
#7966=CARTESIAN_POINT('Ctrl Pts',(0.0789167753987302,0.190427624267694,
0.970684925008453));
#7967=CARTESIAN_POINT('Ctrl Pts',(0.00692518545545543,0.206015968628597,
0.974389829302378));
#7968=CARTESIAN_POINT('Ctrl Pts',(-0.0551388904494672,0.187793009821907,
0.978094733596303));
#7969=CARTESIAN_POINT('Ctrl Pts',(-0.11720296635439,0.169570051015217,0.981799637890228));
#7970=CARTESIAN_POINT('Ctrl Pts',(-0.169339528220959,0.117535789040932,
0.985504542184154));
#7971=CARTESIAN_POINT('Ctrl Pts',(-0.187684350543733,0.0555076241515194,
0.98920944647808));
#7972=CARTESIAN_POINT('Ctrl Pts',(-0.192971863192861,0.0376292985572852,
0.99027730791458));
#7973=CARTESIAN_POINT('Ctrl Pts',(-0.195452091727079,0.0189207190229355,
0.99134516935108));
#7974=CARTESIAN_POINT('Ctrl Pts',(-0.195294337528581,0.000171262189333537,
0.99241303078758));
#7975=CARTESIAN_POINT('Origin',(0.,0.,0.));
#7976=CARTESIAN_POINT('',(-0.195106169435837,-7.43721989362317E-5,1.07258696921242));
#7977=CARTESIAN_POINT('',(-0.195118116536412,-8.83829588442778E-5,1.06241303078758));
#7978=CARTESIAN_POINT('',(-0.1954,-2.39295984553393E-17,0.));
#7979=CARTESIAN_POINT('Ctrl Pts',(-0.195106169435837,-7.43721989362317E-5,
1.07258696921242));
#7980=CARTESIAN_POINT('Ctrl Pts',(-0.194978635044518,0.037194947633429,
1.0704694642039));
#7981=CARTESIAN_POINT('Ctrl Pts',(-0.184712313824149,0.0745293372596056,
1.06835195919538));
#7982=CARTESIAN_POINT('Ctrl Pts',(-0.164756101436382,0.105650071169628,
1.06623445418686));
#7983=CARTESIAN_POINT('Ctrl Pts',(-0.129839604583541,0.160100634558776,
1.06252954989293));
#7984=CARTESIAN_POINT('Ctrl Pts',(-0.0652594983148889,0.195529368597717,
1.05882464559901));
#7985=CARTESIAN_POINT('Ctrl Pts',(-0.000575733727790552,0.195719643953635,
1.05511974130508));
#7986=CARTESIAN_POINT('Ctrl Pts',(0.0641080308593078,0.195909919309552,
1.05141483701116));
#7987=CARTESIAN_POINT('Ctrl Pts',(0.128895453764853,0.160861735982445,1.04770993271723));
#7988=CARTESIAN_POINT('Ctrl Pts',(0.164131689813376,0.106617535601179,1.04400502842331));
#7989=CARTESIAN_POINT('Ctrl Pts',(0.199367925861899,0.0523733352199126,
1.04030012412938));
#7990=CARTESIAN_POINT('Ctrl Pts',(0.205052975053401,-0.0210668822155132,
1.03659521983546));
#7991=CARTESIAN_POINT('Ctrl Pts',(0.178584646313934,-0.0800876682117171,
1.03289031554153));
#7992=CARTESIAN_POINT('Ctrl Pts',(0.152116317574466,-0.13910845420792,1.0291854112476));
#7993=CARTESIAN_POINT('Ctrl Pts',(0.0934946109040307,-0.183709808764902,
1.02548050695368));
#7994=CARTESIAN_POINT('Ctrl Pts',(0.0295521669181964,-0.193476561704776,
1.02177560265975));
#7995=CARTESIAN_POINT('Ctrl Pts',(-0.0343902770676398,-0.20324331464465,
1.01807069836583));
#7996=CARTESIAN_POINT('Ctrl Pts',(-0.103653458368875,-0.178175465967414,
1.0143657940719));
#7997=CARTESIAN_POINT('Ctrl Pts',(-0.146533863776733,-0.129747205231268,
1.01066088977798));
#7998=CARTESIAN_POINT('Ctrl Pts',(-0.177682935350993,-0.0945680751475137,
1.00796958292279));
#7999=CARTESIAN_POINT('Ctrl Pts',(-0.19491028559363,-0.0470620713416631,
1.00527827606761));
#8000=CARTESIAN_POINT('Ctrl Pts',(-0.195321337055717,0.000175186119862003,
1.00258696921242));
#8001=CARTESIAN_POINT('Ctrl Pts',(-0.195294337528581,0.000171262189333537,
0.99241303078758));
#8002=CARTESIAN_POINT('Ctrl Pts',(-0.194904769586374,-0.0461298022874415,
0.995050073645006));
#8003=CARTESIAN_POINT('Ctrl Pts',(-0.178428147697951,-0.0926801463785582,
0.997687116502431));
#8004=CARTESIAN_POINT('Ctrl Pts',(-0.148414044317209,-0.127592253790654,
1.00032415935986));
#8005=CARTESIAN_POINT('Ctrl Pts',(-0.106245832988932,-0.176641899038874,
1.00402906365378));
#8006=CARTESIAN_POINT('Ctrl Pts',(-0.0373563275533994,-0.20271912173077,
1.00773396794771));
#8007=CARTESIAN_POINT('Ctrl Pts',(0.026721999693282,-0.193887716244123,
1.01143887224163));
#8008=CARTESIAN_POINT('Ctrl Pts',(0.0908003269399634,-0.185056310757476,
1.01514377653556));
#8009=CARTESIAN_POINT('Ctrl Pts',(0.150067475997793,-0.141316277092285,
1.01884868082948));
#8010=CARTESIAN_POINT('Ctrl Pts',(0.177395370914998,-0.0826885370284158,
1.02255358512341));
#8011=CARTESIAN_POINT('Ctrl Pts',(0.204723265832202,-0.0240607969645466,
1.02625848941733));
#8012=CARTESIAN_POINT('Ctrl Pts',(0.200111906608781,0.0494546494980005,
1.02996339371126));
#8013=CARTESIAN_POINT('Ctrl Pts',(0.165672029213017,0.10420791963383,1.03366829800518));
#8014=CARTESIAN_POINT('Ctrl Pts',(0.131232151817251,0.158961189769659,1.03737320229911));
#8015=CARTESIAN_POINT('Ctrl Pts',(0.0669637562491417,0.194952283578771,
1.04107810659304));
#8016=CARTESIAN_POINT('Ctrl Pts',(0.00228411571967282,0.195707165411358,
1.04478301088696));
#8017=CARTESIAN_POINT('Ctrl Pts',(-0.0623955248097952,0.196462047243945,
1.04848791518089));
#8018=CARTESIAN_POINT('Ctrl Pts',(-0.127486410300622,0.161980717100009,
1.05219281947481));
#8019=CARTESIAN_POINT('Ctrl Pts',(-0.163194793062323,0.108046153542432,
1.05589772376874));
#8020=CARTESIAN_POINT('Ctrl Pts',(-0.184126604735147,0.0764303804457572,
1.05806949277502));
#8021=CARTESIAN_POINT('Ctrl Pts',(-0.194962120753271,0.0381301666874187,
1.0602412617813));
#8022=CARTESIAN_POINT('Ctrl Pts',(-0.195118116536412,-8.83829588442778E-5,
1.06241303078758));
#8023=CARTESIAN_POINT('Origin',(0.,0.,0.));
#8024=CARTESIAN_POINT('',(-0.195593625707714,-0.000136366597080911,1.14258696921242));
#8025=CARTESIAN_POINT('',(-0.195617452784838,-0.000124751278337231,1.13241303078758));
#8026=CARTESIAN_POINT('',(-0.1954,-2.39295984553393E-17,0.));
#8027=CARTESIAN_POINT('Ctrl Pts',(-0.195593625707714,-0.000136366597080911,
1.14258696921242));
#8028=CARTESIAN_POINT('Ctrl Pts',(-0.195145973734063,0.0562028893414784,
1.13936555663412));
#8029=CARTESIAN_POINT('Ctrl Pts',(-0.169481039857298,0.112897892820961,
1.13614414405582));
#8030=CARTESIAN_POINT('Ctrl Pts',(-0.12658533900641,0.149273783523079,1.13292273147752));
#8031=CARTESIAN_POINT('Ctrl Pts',(-0.0772515568811993,0.191109217632128,
1.12921782718359));
#8032=CARTESIAN_POINT('Ctrl Pts',(-0.00512664276562529,0.206068565381736,
1.12551292288966));
#8033=CARTESIAN_POINT('Ctrl Pts',(0.0567760025061769,0.187304554237428,
1.12180801859574));
#8034=CARTESIAN_POINT('Ctrl Pts',(0.118678647777978,0.168540543093119,1.11810311430181));
#8035=CARTESIAN_POINT('Ctrl Pts',(0.170359024206009,0.116053173054895,1.11439821000789));
#8036=CARTESIAN_POINT('Ctrl Pts',(0.188161713919774,0.0538672434178332,
1.11069330571396));
#8037=CARTESIAN_POINT('Ctrl Pts',(0.205964403633538,-0.00831868621922783,
1.10698840142004));
#8038=CARTESIAN_POINT('Ctrl Pts',(0.189889406633038,-0.0802031754551247,
1.10328349712611));
#8039=CARTESIAN_POINT('Ctrl Pts',(0.147294656385406,-0.128882872015517,
1.09957859283219));
#8040=CARTESIAN_POINT('Ctrl Pts',(0.104699906137772,-0.17756256857591,1.09587368853826));
#8041=CARTESIAN_POINT('Ctrl Pts',(0.0355854026430044,-0.203037472460795,
1.09216878424434));
#8042=CARTESIAN_POINT('Ctrl Pts',(-0.0284133944896331,-0.193647074628664,
1.08846387995041));
#8043=CARTESIAN_POINT('Ctrl Pts',(-0.0924121916222716,-0.184256676796532,
1.08475897565649));
#8044=CARTESIAN_POINT('Ctrl Pts',(-0.15129528239278,-0.140000977247382,
1.08105407136256));
#8045=CARTESIAN_POINT('Ctrl Pts',(-0.178110384059518,-0.0811369311031284,
1.07734916706864));
#8046=CARTESIAN_POINT('Ctrl Pts',(-0.189599553508132,-0.0559161055777398,
1.07576176778323));
#8047=CARTESIAN_POINT('Ctrl Pts',(-0.1952017762943,-0.0280135229595192,
1.07417436849783));
#8048=CARTESIAN_POINT('Ctrl Pts',(-0.195106169435837,-7.43721989362317E-5,
1.07258696921242));
#8049=CARTESIAN_POINT('Ctrl Pts',(-0.195118116536412,-8.83829588442778E-5,
1.06241303078758));
#8050=CARTESIAN_POINT('Ctrl Pts',(-0.195228239960756,-0.0270683273893077,
1.06394616607522));
#8051=CARTESIAN_POINT('Ctrl Pts',(-0.190016233850183,-0.0540075745812006,
1.06547930136287));
#8052=CARTESIAN_POINT('Ctrl Pts',(-0.179276917571505,-0.0785257830526336,
1.06701243665051));
#8053=CARTESIAN_POINT('Ctrl Pts',(-0.153324779286411,-0.137775359118912,
1.07071734094444));
#8054=CARTESIAN_POINT('Ctrl Pts',(-0.0950946226836461,-0.182886714280253,
1.07442224523836));
#8055=CARTESIAN_POINT('Ctrl Pts',(-0.0312398659909398,-0.193211238158751,
1.07812714953229));
#8056=CARTESIAN_POINT('Ctrl Pts',(0.0326148907017665,-0.203535762037249,
1.08183205382621));
#8057=CARTESIAN_POINT('Ctrl Pts',(0.102094247484414,-0.179073454632905,
1.08553695812014));
#8058=CARTESIAN_POINT('Ctrl Pts',(0.145395742152504,-0.131021333918916,
1.08924186241407));
#8059=CARTESIAN_POINT('Ctrl Pts',(0.188697236820593,-0.0829692132049272,
1.09294676670799));
#8060=CARTESIAN_POINT('Ctrl Pts',(0.205820869374125,-0.0113272791812923,
1.09665167100191));
#8061=CARTESIAN_POINT('Ctrl Pts',(0.188928719280947,0.0511121395446363,
1.10035657529584));
#8062=CARTESIAN_POINT('Ctrl Pts',(0.172036569187769,0.113551558270567,1.10406147958977));
#8063=CARTESIAN_POINT('Ctrl Pts',(0.12112863644788,0.166788461698791,1.10776638388369));
#8064=CARTESIAN_POINT('Ctrl Pts',(0.0595067718820099,0.186454970108474,
1.11147128817762));
#8065=CARTESIAN_POINT('Ctrl Pts',(-0.00211509268385834,0.206121478518155,
1.11517619247154));
#8066=CARTESIAN_POINT('Ctrl Pts',(-0.0744508890757059,0.192217591909296,
1.11888109676547));
#8067=CARTESIAN_POINT('Ctrl Pts',(-0.124390690297799,0.151107471506893,
1.12258600105939));
#8068=CARTESIAN_POINT('Ctrl Pts',(-0.168544769350431,0.114760120061932,
1.12586167763545));
#8069=CARTESIAN_POINT('Ctrl Pts',(-0.195191579266694,0.0571452672802262,
1.12913735421152));
#8070=CARTESIAN_POINT('Ctrl Pts',(-0.195617452784838,-0.000124751278337231,
1.13241303078758));
#8071=CARTESIAN_POINT('Origin',(0.,0.,0.));
#8072=CARTESIAN_POINT('',(-0.195527484430252,0.000159769955907059,1.21258696921242));
#8073=CARTESIAN_POINT('',(-0.195499582979996,0.000166550639662629,1.20241303078758));
#8074=CARTESIAN_POINT('',(-0.1954,-2.39295984553393E-17,0.));
#8075=CARTESIAN_POINT('Ctrl Pts',(-0.195527484430252,0.000159769955907059,
1.21258696921242));
#8076=CARTESIAN_POINT('Ctrl Pts',(-0.195623513973876,0.0110197689033327,
1.21196655335827));
#8077=CARTESIAN_POINT('Ctrl Pts',(-0.194796702694689,0.0218651394014599,
1.21134613750411));
#8078=CARTESIAN_POINT('Ctrl Pts',(-0.192995482122666,0.0325461883928473,
1.21072572164995));
#8079=CARTESIAN_POINT('Ctrl Pts',(-0.182239229220893,0.0963296394548849,
1.20702081735602));
#8080=CARTESIAN_POINT('Ctrl Pts',(-0.136734990958994,0.154253292839981,
1.2033159130621));
#8081=CARTESIAN_POINT('Ctrl Pts',(-0.077311210265647,0.179804024609917,
1.19961100876817));
#8082=CARTESIAN_POINT('Ctrl Pts',(-0.0178874295722999,0.205354756379854,
1.19590610447425));
#8083=CARTESIAN_POINT('Ctrl Pts',(0.0554558935524948,0.19853256653463,1.19220120018032));
#8084=CARTESIAN_POINT('Ctrl Pts',(0.109147661596632,0.162460144240518,1.1884962958864));
#8085=CARTESIAN_POINT('Ctrl Pts',(0.162839429640769,0.126387721946406,1.18479139159247));
#8086=CARTESIAN_POINT('Ctrl Pts',(0.196879642604248,0.0610650672034059,
1.18108648729854));
#8087=CARTESIAN_POINT('Ctrl Pts',(0.195687232435581,-0.00360798563825114,
1.17738158300462));
#8088=CARTESIAN_POINT('Ctrl Pts',(0.194494822266914,-0.0682810384799082,
1.17367667871069));
#8089=CARTESIAN_POINT('Ctrl Pts',(0.158069788966098,-0.132304489420224,
1.16997177441677));
#8090=CARTESIAN_POINT('Ctrl Pts',(0.103084793284309,-0.166373182611243,
1.16626687012285));
#8091=CARTESIAN_POINT('Ctrl Pts',(0.0480997976025185,-0.200441875802263,
1.16256196582892));
#8092=CARTESIAN_POINT('Ctrl Pts',(-0.0254451604602465,-0.204555811243987,
1.15885706153499));
#8093=CARTESIAN_POINT('Ctrl Pts',(-0.083886689971347,-0.17683193643772,
1.15515215724107));
#8094=CARTESIAN_POINT('Ctrl Pts',(-0.142328219482446,-0.149108061631455,
1.15144725294714));
#8095=CARTESIAN_POINT('Ctrl Pts',(-0.18566632044188,-0.0895463765772016,
1.14774234865322));
#8096=CARTESIAN_POINT('Ctrl Pts',(-0.194064045854175,-0.0254097738158312,
1.14403744435929));
#8097=CARTESIAN_POINT('Ctrl Pts',(-0.195159952885721,-0.0170399176351585,
1.14355395264367));
#8098=CARTESIAN_POINT('Ctrl Pts',(-0.195660812389172,-0.00859214891261325,
1.14307046092805));
#8099=CARTESIAN_POINT('Ctrl Pts',(-0.195593625707714,-0.000136366597080911,
1.14258696921242));
#8100=CARTESIAN_POINT('Ctrl Pts',(-0.195617452784838,-0.000124751278337231,
1.13241303078758));
#8101=CARTESIAN_POINT('Ctrl Pts',(-0.195673257048185,-0.00762911832956361,
1.13284225850544));
#8102=CARTESIAN_POINT('Ctrl Pts',(-0.19527884452345,-0.0151275645336468,
1.13327148622331));
#8103=CARTESIAN_POINT('Ctrl Pts',(-0.194414610465335,-0.0225714646308396,
1.13370071394117));
#8104=CARTESIAN_POINT('Ctrl Pts',(-0.186954923358439,-0.0868239261702202,
1.1374056182351));
#8105=CARTESIAN_POINT('Ctrl Pts',(-0.144491743092308,-0.147012495053033,
1.14111052252902));
#8106=CARTESIAN_POINT('Ctrl Pts',(-0.0864615432906266,-0.175587338124856,
1.14481542682294));
#8107=CARTESIAN_POINT('Ctrl Pts',(-0.028431343488945,-0.204162181196678,
1.14852033111687));
#8108=CARTESIAN_POINT('Ctrl Pts',(0.0451658758482873,-0.20112329845751,
1.1522252354108));
#8109=CARTESIAN_POINT('Ctrl Pts',(0.100642802478808,-0.167861663542278,
1.15593013970472));
#8110=CARTESIAN_POINT('Ctrl Pts',(0.156119729109329,-0.134600028627046,
1.15963504399865));
#8111=CARTESIAN_POINT('Ctrl Pts',(0.193476363033138,-0.0711156415357493,
1.16333994829257));
#8112=CARTESIAN_POINT('Ctrl Pts',(0.195613626287182,-0.00646691493278147,
1.1670448525865));
#8113=CARTESIAN_POINT('Ctrl Pts',(0.197750889541227,0.0581818116701864,
1.17074975688042));
#8114=CARTESIAN_POINT('Ctrl Pts',(0.164668782125508,0.123994877784826,1.17445466117435));
#8115=CARTESIAN_POINT('Ctrl Pts',(0.111509822903934,0.160847975349094,1.17815956546828));
#8116=CARTESIAN_POINT('Ctrl Pts',(0.0583508636823605,0.197701072913362,
1.1818644697622));
#8117=CARTESIAN_POINT('Ctrl Pts',(-0.0148849473450669,0.205594201927258,
1.18556937405613));
#8118=CARTESIAN_POINT('Ctrl Pts',(-0.0746757236775608,0.180914477229441,
1.18927427835005));
#8119=CARTESIAN_POINT('Ctrl Pts',(-0.134466500010055,0.156234752531623,
1.19297918264398));
#8120=CARTESIAN_POINT('Ctrl Pts',(-0.180812241647615,0.098982174122092,
1.1966840869379));
#8121=CARTESIAN_POINT('Ctrl Pts',(-0.192499328242851,0.0353626979177265,
1.20038899123183));
#8122=CARTESIAN_POINT('Ctrl Pts',(-0.194627599644181,0.0237773031600198,
1.20106367108374));
#8123=CARTESIAN_POINT('Ctrl Pts',(-0.195606518663776,0.011980768958621,
1.20173835093566));
#8124=CARTESIAN_POINT('Ctrl Pts',(-0.195499582979996,0.000166550639662629,
1.20241303078758));
#8125=CARTESIAN_POINT('Origin',(0.,0.,0.));
#8126=CARTESIAN_POINT('',(-0.195085605073228,3.67867518197285E-5,1.28258696921242));
#8127=CARTESIAN_POINT('',(-0.19508137714814,2.13056907460231E-5,1.27241303078758));
#8128=CARTESIAN_POINT('',(-0.1954,-2.39295984553393E-17,0.));
#8129=CARTESIAN_POINT('Ctrl Pts',(-0.195085605073228,3.67867518197285E-5,
1.28258696921242));
#8130=CARTESIAN_POINT('Ctrl Pts',(-0.195136667969355,0.0303938707492628,
1.28086264578848));
#8131=CARTESIAN_POINT('Ctrl Pts',(-0.188480024483457,0.0607297539874398,
1.27913832236455));
#8132=CARTESIAN_POINT('Ctrl Pts',(-0.174998421369655,0.0876473788358303,
1.27741399894061));
#8133=CARTESIAN_POINT('Ctrl Pts',(-0.146031669209427,0.145482946397307,
1.27370909464668));
#8134=CARTESIAN_POINT('Ctrl Pts',(-0.0855572231025935,0.187537989963383,
1.27000419035276));
#8135=CARTESIAN_POINT('Ctrl Pts',(-0.0212557694531386,0.194562850420161,
1.26629928605883));
#8136=CARTESIAN_POINT('Ctrl Pts',(0.0430456841963182,0.201587710876938,
1.2625943817649));
#8137=CARTESIAN_POINT('Ctrl Pts',(0.111174145388397,0.173582388224419,1.25888947747098));
#8138=CARTESIAN_POINT('Ctrl Pts',(0.151945491062064,0.123365628294801,1.25518457317705));
#8139=CARTESIAN_POINT('Ctrl Pts',(0.192716836735728,0.0731488683651866,
1.25147966888313));
#8140=CARTESIAN_POINT('Ctrl Pts',(0.206131066890981,0.000720671158477647,
1.2477747645892));
#8141=CARTESIAN_POINT('Ctrl Pts',(0.186048148469522,-0.0607667421351959,
1.24406986029528));
#8142=CARTESIAN_POINT('Ctrl Pts',(0.165965230048063,-0.122254155428872,
1.24036495600135));
#8143=CARTESIAN_POINT('Ctrl Pts',(0.112385163049889,-0.172800784809512,
1.23666005170743));
#8144=CARTESIAN_POINT('Ctrl Pts',(0.0498329018575594,-0.189270157159331,
1.2329551474135));
#8145=CARTESIAN_POINT('Ctrl Pts',(-0.0127193593347688,-0.205739529509149,
1.22925024311958));
#8146=CARTESIAN_POINT('Ctrl Pts',(-0.0842438147212514,-0.188131644828148,
1.22554533882565));
#8147=CARTESIAN_POINT('Ctrl Pts',(-0.132001908643669,-0.144506078118158,
1.22184043453172));
#8148=CARTESIAN_POINT('Ctrl Pts',(-0.171762527791251,-0.108185961451209,
1.21875594609196));
#8149=CARTESIAN_POINT('Ctrl Pts',(-0.195050059465688,-0.0538323080748223,
1.21567145765219));
#8150=CARTESIAN_POINT('Ctrl Pts',(-0.195527484430252,0.000159769955907059,
1.21258696921242));
#8151=CARTESIAN_POINT('Ctrl Pts',(-0.195499582979996,0.000166550639662629,
1.20241303078758));
#8152=CARTESIAN_POINT('Ctrl Pts',(-0.195019297224031,-0.0528952578782005,
1.20544325522959));
#8153=CARTESIAN_POINT('Ctrl Pts',(-0.172634890521839,-0.106313794647688,
1.2084734796716));
#8154=CARTESIAN_POINT('Ctrl Pts',(-0.134099291878761,-0.142561887247553,
1.2115037041136));
#8155=CARTESIAN_POINT('Ctrl Pts',(-0.0869837373665235,-0.186880622209269,
1.21520860840753));
#8156=CARTESIAN_POINT('Ctrl Pts',(-0.0157241967891372,-0.205531718133499,
1.21891351270145));
#8157=CARTESIAN_POINT('Ctrl Pts',(0.0470620324162366,-0.189978095797443,
1.22261841699538));
#8158=CARTESIAN_POINT('Ctrl Pts',(0.10984826162161,-0.174424473461387,1.2263233212893));
#8159=CARTESIAN_POINT('Ctrl Pts',(0.16416117945497,-0.124666132865044,1.23002822558323));
#8160=CARTESIAN_POINT('Ctrl Pts',(0.185140387136073,-0.0634787273744072,
1.23373312987716));
#8161=CARTESIAN_POINT('Ctrl Pts',(0.206119594817175,-0.00229132188377159,
1.23743803417108));
#8162=CARTESIAN_POINT('Ctrl Pts',(0.19376509234602,0.0703251485011587,1.24114293846501));
#8163=CARTESIAN_POINT('Ctrl Pts',(0.153731848566424,0.12113228518574,1.24484784275893));
#8164=CARTESIAN_POINT('Ctrl Pts',(0.113698604786827,0.171939421870322,1.24855274705286));
#8165=CARTESIAN_POINT('Ctrl Pts',(0.0459866196987903,0.200937224854556,
1.25225765134678));
#8166=CARTESIAN_POINT('Ctrl Pts',(-0.0184106153029644,0.194852664908991,
1.25596255564071));
#8167=CARTESIAN_POINT('Ctrl Pts',(-0.0828078503047191,0.188768104963426,
1.25966745993463));
#8168=CARTESIAN_POINT('Ctrl Pts',(-0.14389033522019,0.147601182088061,1.26337236422856));
#8169=CARTESIAN_POINT('Ctrl Pts',(-0.173699068875,0.0901950400516983,1.26707726852248));
#8170=CARTESIAN_POINT('Ctrl Pts',(-0.188009138590469,0.0626364760365528,
1.26885585594418));
#8171=CARTESIAN_POINT('Ctrl Pts',(-0.195111844846784,0.0313354139177859,
1.27063444336588));
#8172=CARTESIAN_POINT('Ctrl Pts',(-0.19508137714814,2.13056907460231E-5,
1.27241303078758));
#8173=CARTESIAN_POINT('Origin',(0.,0.,0.));
#8174=CARTESIAN_POINT('',(-0.195392498133114,-0.000178699422991063,1.35258696921242));
#8175=CARTESIAN_POINT('',(-0.195421369810842,-0.000177481533986374,1.34241303078758));
#8176=CARTESIAN_POINT('',(-0.1954,-2.39295984553393E-17,0.));
#8177=CARTESIAN_POINT('Ctrl Pts',(-0.195392498133114,-0.000178699422991063,
1.35258696921242));
#8178=CARTESIAN_POINT('Ctrl Pts',(-0.194938084649759,0.0494157798589555,
1.3497587382187));
#8179=CARTESIAN_POINT('Ctrl Pts',(-0.17572581092509,0.099323482715635,1.34693050722498));
#8180=CARTESIAN_POINT('Ctrl Pts',(-0.141651466296104,0.135060625627259,
1.34410227623126));
#8181=CARTESIAN_POINT('Ctrl Pts',(-0.0970150182800354,0.181875293354148,
1.34039737193734));
#8182=CARTESIAN_POINT('Ctrl Pts',(-0.0268748485034288,0.204372891114381,
1.33669246764341));
#8183=CARTESIAN_POINT('Ctrl Pts',(0.0366641099768968,0.192255698324562,
1.33298756334949));
#8184=CARTESIAN_POINT('Ctrl Pts',(0.100203068457222,0.180138505534742,1.32928265905556));
#8185=CARTESIAN_POINT('Ctrl Pts',(0.157140815641268,0.133406522194869,1.32557775476164));
#8186=CARTESIAN_POINT('Ctrl Pts',(0.181415501841872,0.0734501612668376,
1.32187285046771));
#8187=CARTESIAN_POINT('Ctrl Pts',(0.205690188042477,0.0134938003388052,
1.31816794617379));
#8188=CARTESIAN_POINT('Ctrl Pts',(0.197301813259641,-0.0596869381773843,
1.31446304187986));
#8189=CARTESIAN_POINT('Ctrl Pts',(0.160089949192665,-0.112595375864876,
1.31075813758593));
#8190=CARTESIAN_POINT('Ctrl Pts',(0.12287808512569,-0.165503813552367,1.30705323329201));
#8191=CARTESIAN_POINT('Ctrl Pts',(0.0568427317745747,-0.19813995041116,
1.30334832899808));
#8192=CARTESIAN_POINT('Ctrl Pts',(-0.00779005629774907,-0.19556539960213,
1.29964342470416));
#8193=CARTESIAN_POINT('Ctrl Pts',(-0.0724228443700711,-0.1929908487931,
1.29593852041023));
#8194=CARTESIAN_POINT('Ctrl Pts',(-0.135653067163603,-0.155205610316251,
1.29223361611631));
#8195=CARTESIAN_POINT('Ctrl Pts',(-0.168538649453556,-0.0995049452993885,
1.28852871182238));
#8196=CARTESIAN_POINT('Ctrl Pts',(-0.186118740601559,-0.0697282863560552,
1.2865481309524));
#8197=CARTESIAN_POINT('Ctrl Pts',(-0.195026953550068,-0.0348317645878951,
1.28456755008241));
#8198=CARTESIAN_POINT('Ctrl Pts',(-0.195085605073228,3.67867518197285E-5,
1.28258696921242));
#8199=CARTESIAN_POINT('Ctrl Pts',(-0.19508137714814,2.13056907460231E-5,
1.27241303078758));
#8200=CARTESIAN_POINT('Ctrl Pts',(-0.1950483788028,-0.0338937520008573,
1.27433934765981));
#8201=CARTESIAN_POINT('Ctrl Pts',(-0.186648032317626,-0.0678241130245367,
1.27626566453203));
#8202=CARTESIAN_POINT('Ctrl Pts',(-0.169974591739146,-0.0970316955488254,
1.27819198140426));
#8203=CARTESIAN_POINT('Ctrl Pts',(-0.137906398554337,-0.153206927915627,
1.28189688569818));
#8204=CARTESIAN_POINT('Ctrl Pts',(-0.0752350297905721,-0.19191203145187,
1.28560178999211));
#8205=CARTESIAN_POINT('Ctrl Pts',(-0.0106467590218702,-0.195430699482706,
1.28930669428604));
#8206=CARTESIAN_POINT('Ctrl Pts',(0.0539415117468317,-0.198949367513541,
1.29301159857996));
#8207=CARTESIAN_POINT('Ctrl Pts',(0.120446684520471,-0.16728160003897,1.29671650287389));
#8208=CARTESIAN_POINT('Ctrl Pts',(0.158427656481215,-0.114922536692502,
1.30042140716781));
#8209=CARTESIAN_POINT('Ctrl Pts',(0.19640862844196,-0.0625634733460332,
1.30412631146174));
#8210=CARTESIAN_POINT('Ctrl Pts',(0.205865399589811,0.0104868858723325,
1.30783121575566));
#8211=CARTESIAN_POINT('Ctrl Pts',(0.182469366136063,0.0707915404541595,
1.31153612004959));
#8212=CARTESIAN_POINT('Ctrl Pts',(0.159073332682314,0.131096195035986,1.31524102434351));
#8213=CARTESIAN_POINT('Ctrl Pts',(0.102824494626968,0.178655144981275,1.31894592863744));
#8214=CARTESIAN_POINT('Ctrl Pts',(0.039469370492038,0.19169945375752,1.32265083293136));
#8215=CARTESIAN_POINT('Ctrl Pts',(-0.0238857536428916,0.204743762533765,
1.32635573722529));
#8216=CARTESIAN_POINT('Ctrl Pts',(-0.0943471638574042,0.183273430140967,
1.33006064151922));
#8217=CARTESIAN_POINT('Ctrl Pts',(-0.139662887206028,0.137115971772969,
1.33376554581314));
#8218=CARTESIAN_POINT('Ctrl Pts',(-0.174919491756342,0.101204479326771,
1.33664804080462));
#8219=CARTESIAN_POINT('Ctrl Pts',(-0.194954975303473,0.0503494407490454,
1.3395305357961));
#8220=CARTESIAN_POINT('Ctrl Pts',(-0.195421369810842,-0.000177481533986374,
1.34241303078758));
#8221=CARTESIAN_POINT('Origin',(0.,0.,0.));
#8222=CARTESIAN_POINT('',(-0.195688377393879,7.16972608892641E-5,1.42258696921242));
#8223=CARTESIAN_POINT('',(-0.195672555088735,8.72824817547956E-5,1.41241303078758));
#8224=CARTESIAN_POINT('',(-0.1954,-2.39295984553393E-17,0.));
#8225=CARTESIAN_POINT('Ctrl Pts',(-0.195688377393879,7.16972608892641E-5,
1.42258696921242));
#8226=CARTESIAN_POINT('Ctrl Pts',(-0.195707099359798,0.0040407295163859,
1.42235973494285));
#8227=CARTESIAN_POINT('Ctrl Pts',(-0.195596806193923,0.00800870147258908,
1.42213250067327));
#8228=CARTESIAN_POINT('Ctrl Pts',(-0.195354201126062,0.0119685672100241,
1.4219052664037));
#8229=CARTESIAN_POINT('Ctrl Pts',(-0.191398686144431,0.0765315558885256,
1.41820036210977));
#8230=CARTESIAN_POINT('Ctrl Pts',(-0.152270508849115,0.138939656827576,
1.41449545781585));
#8231=CARTESIAN_POINT('Ctrl Pts',(-0.0958796274951682,0.170627100807728,
1.41079055352192));
#8232=CARTESIAN_POINT('Ctrl Pts',(-0.0394887461412211,0.20231454478788,
1.40708564922799));
#8233=CARTESIAN_POINT('Ctrl Pts',(0.034164839271357,0.203281331809134,1.40338074493407));
#8234=CARTESIAN_POINT('Ctrl Pts',(0.0913680163193032,0.173084938953504,
1.39967584064014));
#8235=CARTESIAN_POINT('Ctrl Pts',(0.148571193367249,0.142888546097875,1.39597093634622));
#8236=CARTESIAN_POINT('Ctrl Pts',(0.189323962050564,0.0815289733653608,
1.39226603205229));
#8237=CARTESIAN_POINT('Ctrl Pts',(0.194972747468802,0.0170920520456009,
1.38856112775837));
#8238=CARTESIAN_POINT('Ctrl Pts',(0.200621532887041,-0.0473448692741589,
1.38485622346444));
#8239=CARTESIAN_POINT('Ctrl Pts',(0.171166335040203,-0.114859139181165,
1.38115131917052));
#8240=CARTESIAN_POINT('Ctrl Pts',(0.120089544376728,-0.154547765529148,
1.37744641487659));
#8241=CARTESIAN_POINT('Ctrl Pts',(0.0690127537132543,-0.194236391877132,
1.37374151058267));
#8242=CARTESIAN_POINT('Ctrl Pts',(-0.00368562976685627,-0.206099374666093,
1.37003660628874));
#8243=CARTESIAN_POINT('Ctrl Pts',(-0.0647297137696226,-0.184706726065852,
1.36633170199482));
#8244=CARTESIAN_POINT('Ctrl Pts',(-0.125773797772389,-0.16331407746561,
1.36262679770089));
#8245=CARTESIAN_POINT('Ctrl Pts',(-0.175163582297811,-0.108665797476165,
1.35892189340696));
#8246=CARTESIAN_POINT('Ctrl Pts',(-0.190292111432757,-0.0457757886346702,
1.35521698911304));
#8247=CARTESIAN_POINT('Ctrl Pts',(-0.193871900952753,-0.030894434832521,
1.35434031581283));
#8248=CARTESIAN_POINT('Ctrl Pts',(-0.195533353731187,-0.0155516148321636,
1.35346364251263));
#8249=CARTESIAN_POINT('Ctrl Pts',(-0.195392498133114,-0.000178699422991063,
1.35258696921242));
#8250=CARTESIAN_POINT('Ctrl Pts',(-0.195421369810842,-0.000177481533986374,
1.34241303078758));
#8251=CARTESIAN_POINT('Ctrl Pts',(-0.19555443758116,-0.0145933993525209,
1.34323544009003));
#8252=CARTESIAN_POINT('Ctrl Pts',(-0.194094528316993,-0.0289826076128833,
1.34405784939247));
#8253=CARTESIAN_POINT('Ctrl Pts',(-0.190940659847886,-0.0429904198028263,
1.34488025869492));
#8254=CARTESIAN_POINT('Ctrl Pts',(-0.176732672658387,-0.106094768667428,
1.34858516298884));
#8255=CARTESIAN_POINT('Ctrl Pts',(-0.128146661796655,-0.161458882053436,
1.35229006728277));
#8256=CARTESIAN_POINT('Ctrl Pts',(-0.0674216756023477,-0.183741202338891,
1.35599497157669));
#8257=CARTESIAN_POINT('Ctrl Pts',(-0.00669668940803995,-0.206023522624345,
1.35969987587062));
#8258=CARTESIAN_POINT('Ctrl Pts',(0.0661672721188413,-0.195224049809246,
1.36340478016454));
#8259=CARTESIAN_POINT('Ctrl Pts',(0.117818527416568,-0.156285976259422,
1.36710968445847));
#8260=CARTESIAN_POINT('Ctrl Pts',(0.169469782714294,-0.117347902709599,
1.3708145887524));
#8261=CARTESIAN_POINT('Ctrl Pts',(0.199908331782865,-0.0502712284250506,
1.37451949304632));
#8262=CARTESIAN_POINT('Ctrl Pts',(0.195201679401558,0.0142413530530136,
1.37822439734025));
#8263=CARTESIAN_POINT('Ctrl Pts',(0.190495027020252,0.0787539345310777,
1.38192930163417));
#8264=CARTESIAN_POINT('Ctrl Pts',(0.150643173189068,0.140702423202659,1.3856342059281));
#8265=CARTESIAN_POINT('Ctrl Pts',(0.0938873212514722,0.171731426029694,
1.38933911022202));
#8266=CARTESIAN_POINT('Ctrl Pts',(0.0371314693138761,0.202760428856729,
1.39304401451595));
#8267=CARTESIAN_POINT('Ctrl Pts',(-0.0365283807301298,0.202869945839216,
1.39674891880987));
#8268=CARTESIAN_POINT('Ctrl Pts',(-0.0933762489767357,0.172009848279114,
1.4004538231038));
#8269=CARTESIAN_POINT('Ctrl Pts',(-0.150224117223341,0.141149750719013,
1.40415872739772));
#8270=CARTESIAN_POINT('Ctrl Pts',(-0.190260003672545,0.0793200386163227,
1.40786363169165));
#8271=CARTESIAN_POINT('Ctrl Pts',(-0.195158468588232,0.014821737963731,
1.41156853598557));
#8272=CARTESIAN_POINT('Ctrl Pts',(-0.195530653475337,0.009921163363317,
1.41185003425291));
#8273=CARTESIAN_POINT('Ctrl Pts',(-0.195699991939521,0.00500518314638453,
1.41213153252024));
#8274=CARTESIAN_POINT('Ctrl Pts',(-0.195672555088735,8.72824817547956E-5,
1.41241303078758));
#8275=CARTESIAN_POINT('Origin',(0.,0.,0.));
#8276=CARTESIAN_POINT('',(-0.195179950177078,0.000133868047100166,1.49258696921242));
#8277=CARTESIAN_POINT('',(-0.195160806943041,0.000122850585401665,1.48241303078758));
#8278=CARTESIAN_POINT('',(-0.1954,-2.39295984553393E-17,0.));
#8279=CARTESIAN_POINT('Ctrl Pts',(-0.195179950177078,0.000133868047100166,
1.49258696921242));
#8280=CARTESIAN_POINT('Ctrl Pts',(-0.19532758311484,0.0235405577971841,
1.49125582737307));
#8281=CARTESIAN_POINT('Ctrl Pts',(-0.191434166902591,0.0468997728483757,
1.48992468553371));
#8282=CARTESIAN_POINT('Ctrl Pts',(-0.183280900003334,0.0686631064883505,
1.48859354369435));
#8283=CARTESIAN_POINT('Ctrl Pts',(-0.160588296817507,0.129235966471356,
1.48488863940043));
#8284=CARTESIAN_POINT('Ctrl Pts',(-0.104896775936504,0.177446336966025,
1.4811837351065));
#8285=CARTESIAN_POINT('Ctrl Pts',(-0.041697757689242,0.191227109747421,
1.47747883081258));
#8286=CARTESIAN_POINT('Ctrl Pts',(0.02150126055802,0.205007882528817,1.47377392651865));
#8287=CARTESIAN_POINT('Ctrl Pts',(0.0922077761715412,0.184359057596941,
1.47006902222473));
#8288=CARTESIAN_POINT('Ctrl Pts',(0.138057625253759,0.138732125363795,1.4663641179308));
#8289=CARTESIAN_POINT('Ctrl Pts',(0.183907474335976,0.0931051931306484,
1.46265921363688));
#8290=CARTESIAN_POINT('Ctrl Pts',(0.20490065688689,0.0225001535962327,1.45895430934295));
#8291=CARTESIAN_POINT('Ctrl Pts',(0.191428061286251,-0.0407652775146975,
1.45524940504902));
#8292=CARTESIAN_POINT('Ctrl Pts',(0.177955465685611,-0.104030708625628,
1.4515445007551));
#8293=CARTESIAN_POINT('Ctrl Pts',(0.130017091933419,-0.159956531313072,
1.44783959646117));
#8294=CARTESIAN_POINT('Ctrl Pts',(0.0695555484531877,-0.182944079374106,
1.44413469216725));
#8295=CARTESIAN_POINT('Ctrl Pts',(0.00909400497295641,-0.205931627435139,
1.44042978787332));
#8296=CARTESIAN_POINT('Ctrl Pts',(-0.063890708235314,-0.195980900869761,
1.4367248835794));
#8297=CARTESIAN_POINT('Ctrl Pts',(-0.115991638505476,-0.157646599378095,
1.43301997928547));
#8298=CARTESIAN_POINT('Ctrl Pts',(-0.164897043089976,-0.121663469821813,
1.42954230926112));
#8299=CARTESIAN_POINT('Ctrl Pts',(-0.195401850102924,-0.0606717131691646,
1.42606463923677));
#8300=CARTESIAN_POINT('Ctrl Pts',(-0.195688377393879,7.16972608892641E-5,
1.42258696921242));
#8301=CARTESIAN_POINT('Ctrl Pts',(-0.195672555088735,8.72824817547956E-5,
1.41241303078758));
#8302=CARTESIAN_POINT('Ctrl Pts',(-0.195338885254029,-0.0597211523368212,
1.41583643681417));
#8303=CARTESIAN_POINT('Ctrl Pts',(-0.16590233426085,-0.119813619535752,
1.41925984284076));
#8304=CARTESIAN_POINT('Ctrl Pts',(-0.118282735433092,-0.155934942448556,
1.42268324886735));
#8305=CARTESIAN_POINT('Ctrl Pts',(-0.0667474939800966,-0.195026433005756,
1.42638815316128));
#8306=CARTESIAN_POINT('Ctrl Pts',(0.00608403230806285,-0.206042524917664,
1.4300930574552));
#8307=CARTESIAN_POINT('Ctrl Pts',(0.0668750083003318,-0.183940873768719,
1.43379796174913));
#8308=CARTESIAN_POINT('Ctrl Pts',(0.127665984292602,-0.161839222619775,
1.43750286604305));
#8309=CARTESIAN_POINT('Ctrl Pts',(0.176416409988978,-0.106619828409975,
1.44120777033698));
#8310=CARTESIAN_POINT('Ctrl Pts',(0.190811980213718,-0.0435580071271506,
1.4449126746309));
#8311=CARTESIAN_POINT('Ctrl Pts',(0.205207550438459,0.019503814155676,1.44861757892483));
#8312=CARTESIAN_POINT('Ctrl Pts',(0.185248265191562,0.0904080625115289,
1.45232248321875));
#8313=CARTESIAN_POINT('Ctrl Pts',(0.140069995098299,0.136700066756136,1.45602738751268));
#8314=CARTESIAN_POINT('Ctrl Pts',(0.0948917250050361,0.182992071000741,
1.4597322918066));
#8315=CARTESIAN_POINT('Ctrl Pts',(0.0244944700654076,0.204671831134102,
1.46343719610053));
#8316=CARTESIAN_POINT('Ctrl Pts',(-0.0388991622701212,0.191815971578626,
1.46714210039445));
#8317=CARTESIAN_POINT('Ctrl Pts',(-0.10229279460565,0.178960112023149,1.47084700468838));
#8318=CARTESIAN_POINT('Ctrl Pts',(-0.15868280433708,0.131568632778834,1.47455190898231));
#8319=CARTESIAN_POINT('Ctrl Pts',(-0.182258055088965,0.0713338147946472,
1.47825681327623));
#8320=CARTESIAN_POINT('Ctrl Pts',(-0.191073745701187,0.0488097057185394,
1.47964221911335));
#8321=CARTESIAN_POINT('Ctrl Pts',(-0.195300951932749,0.0244897139044186,
1.48102762495046));
#8322=CARTESIAN_POINT('Ctrl Pts',(-0.195160806943041,0.000122850585401665,
1.48241303078758));
#8323=CARTESIAN_POINT('Origin',(0.,0.,0.));
#8324=CARTESIAN_POINT('',(-0.195203598247727,-0.000145069483009505,1.56258696921242));
#8325=CARTESIAN_POINT('',(-0.195226188848194,-0.00015379427405286,1.55241303078758));
#8326=CARTESIAN_POINT('',(-0.1954,-2.39295984553393E-17,0.));
#8327=CARTESIAN_POINT('Ctrl Pts',(-0.195203598247727,-0.000145069483009505,
1.56258696921242));
#8328=CARTESIAN_POINT('Ctrl Pts',(-0.194908648709454,0.0426596016193331,
1.56015191980329));
#8329=CARTESIAN_POINT('Ctrl Pts',(-0.181052651050772,0.0856379285438176,
1.55771687039415));
#8330=CARTESIAN_POINT('Ctrl Pts',(-0.155131211310912,0.119334897560907,
1.55528182098501));
#8331=CARTESIAN_POINT('Ctrl Pts',(-0.11569198965218,0.170604512351969,1.55157691669109));
#8332=CARTESIAN_POINT('Ctrl Pts',(-0.0483220775946747,0.200388405157253,
1.54787201239716));
#8333=CARTESIAN_POINT('Ctrl Pts',(0.0161416089610767,0.195053733516717,
1.54416710810323));
#8334=CARTESIAN_POINT('Ctrl Pts',(0.0806052955168263,0.189719061876181,
1.54046220380931));
#8335=CARTESIAN_POINT('Ctrl Pts',(0.14216275657082,0.149265825789827,1.53675729951538));
#8336=CARTESIAN_POINT('Ctrl Pts',(0.172637582334195,0.0922104964983205,
1.53305239522146));
#8337=CARTESIAN_POINT('Ctrl Pts',(0.20311240809757,0.0351551672068159,1.52934749092753));
#8338=CARTESIAN_POINT('Ctrl Pts',(0.202504598570326,-0.0385022552898431,
1.52564258663361));
#8339=CARTESIAN_POINT('Ctrl Pts',(0.17109236357496,-0.0950469022377724,
1.52193768233968));
#8340=CARTESIAN_POINT('Ctrl Pts',(0.139680128579593,-0.151591549185703,
1.51823277804576));
#8341=CARTESIAN_POINT('Ctrl Pts',(0.077463468116105,-0.191023420584907,
1.51452787375183));
#8342=CARTESIAN_POINT('Ctrl Pts',(0.0129205242471798,-0.195293549693381,
1.51082296945791));
#8343=CARTESIAN_POINT('Ctrl Pts',(-0.0516224196217455,-0.199563678801854,
1.50711806516398));
#8344=CARTESIAN_POINT('Ctrl Pts',(-0.118491646896106,-0.168672065619597,
1.50341316087006));
#8345=CARTESIAN_POINT('Ctrl Pts',(-0.157079417787961,-0.116758584292797,
1.49970825657613));
#8346=CARTESIAN_POINT('Ctrl Pts',(-0.181802917906106,-0.0834971926121641,
1.49733449412156));
#8347=CARTESIAN_POINT('Ctrl Pts',(-0.194916683322746,-0.0416061777329493,
1.49496073166699));
#8348=CARTESIAN_POINT('Ctrl Pts',(-0.195179950177078,0.000133868047100166,
1.49258696921242));
#8349=CARTESIAN_POINT('Ctrl Pts',(-0.195160806943041,0.000122850585401665,
1.48241303078758));
#8350=CARTESIAN_POINT('Ctrl Pts',(-0.194926170940615,-0.0406730666480617,
1.48473252924439));
#8351=CARTESIAN_POINT('Ctrl Pts',(-0.182449537937005,-0.0816003680531453,
1.4870520277012));
#8352=CARTESIAN_POINT('Ctrl Pts',(-0.158768687450683,-0.114450931246349,
1.48937152615801));
#8353=CARTESIAN_POINT('Ctrl Pts',(-0.120943577288175,-0.166922702579101,
1.49307643045193));
#8354=CARTESIAN_POINT('Ctrl Pts',(-0.0545328651908197,-0.198788088520544,
1.49678133474586));
#8355=CARTESIAN_POINT('Ctrl Pts',(0.0100655830687197,-0.195461494457236,
1.50048623903978));
#8356=CARTESIAN_POINT('Ctrl Pts',(0.074664031328259,-0.192134900393928,
1.50419114333371));
#8357=CARTESIAN_POINT('Ctrl Pts',(0.13745021574998,-0.153616326325868,1.50789604762764));
#8358=CARTESIAN_POINT('Ctrl Pts',(0.169685308723794,-0.0975366996636656,
1.51160095192156));
#8359=CARTESIAN_POINT('Ctrl Pts',(0.201920401697606,-0.0414570730014645,
1.51530585621549));
#8360=CARTESIAN_POINT('Ctrl Pts',(0.203604403223511,0.0321836062548823,
1.51901076050941));
#8361=CARTESIAN_POINT('Ctrl Pts',(0.173966503130547,0.0896781331568551,
1.52271566480334));
#8362=CARTESIAN_POINT('Ctrl Pts',(0.144328603037582,0.147172660058829,1.52642056909726));
#8363=CARTESIAN_POINT('Ctrl Pts',(0.0833688013257482,0.188521034606432,
1.53012547339119));
#8364=CARTESIAN_POINT('Ctrl Pts',(0.0189899439583294,0.194797058002499,
1.53383037768511));
#8365=CARTESIAN_POINT('Ctrl Pts',(-0.0453889134090893,0.201073081398565,
1.53753528197904));
#8366=CARTESIAN_POINT('Ctrl Pts',(-0.113186826432091,0.172276753643094,
1.54124018627296));
#8367=CARTESIAN_POINT('Ctrl Pts',(-0.153370972322708,0.121588883647957,
1.54494509056689));
#8368=CARTESIAN_POINT('Ctrl Pts',(-0.180370572089492,0.0875318650758873,
1.54743440397379));
#8369=CARTESIAN_POINT('Ctrl Pts',(-0.19490406552098,0.0435920118983492,
1.54992371738068));
#8370=CARTESIAN_POINT('Ctrl Pts',(-0.195226188848194,-0.00015379427405286,
1.55241303078758));
#8371=CARTESIAN_POINT('Origin',(0.,0.,0.));
#8372=CARTESIAN_POINT('',(-0.195702834179537,-5.31785447526745E-5,1.63258696921242));
#8373=CARTESIAN_POINT('',(-0.195712283470102,-3.61459064724743E-5,1.62241303078758));
#8374=CARTESIAN_POINT('',(-0.1954,-2.39295984553393E-17,0.));
#8375=CARTESIAN_POINT('Ctrl Pts',(-0.195702834179537,-5.31785447526745E-5,
1.63258696921242));
#8376=CARTESIAN_POINT('Ctrl Pts',(-0.195478917826867,0.061748543580026,
1.62904801223351));
#8377=CARTESIAN_POINT('Ctrl Pts',(-0.163739035867485,0.12374830482208,1.62550905525459));
#8378=CARTESIAN_POINT('Ctrl Pts',(-0.113374270159849,0.15953929097368,1.62197009827567));
#8379=CARTESIAN_POINT('Ctrl Pts',(-0.0606478205747536,0.197008573326304,
1.61826519398174));
#8380=CARTESIAN_POINT('Ctrl Pts',(0.0124911663215799,0.205753509978468,
1.61456028968782));
#8381=CARTESIAN_POINT('Ctrl Pts',(0.0725651228866868,0.181771321828013,
1.61085538539389));
#8382=CARTESIAN_POINT('Ctrl Pts',(0.132639079451794,0.157789133677557,1.60715048109997));
#8383=CARTESIAN_POINT('Ctrl Pts',(0.179648005685674,0.10107982072448,1.60344557680604));
#8384=CARTESIAN_POINT('Ctrl Pts',(0.192074724846121,0.0376006725199113,
1.59974067251212));
#8385=CARTESIAN_POINT('Ctrl Pts',(0.204501444006568,-0.0258784756846574,
1.59603576821819));
#8386=CARTESIAN_POINT('Ctrl Pts',(0.182345956093582,-0.0961274591407182,
1.59233086392426));
#8387=CARTESIAN_POINT('Ctrl Pts',(0.13574938934442,-0.140991538013031,1.58862595963034));
#8388=CARTESIAN_POINT('Ctrl Pts',(0.0891528225952577,-0.185855616885343,
1.58492105533641));
#8389=CARTESIAN_POINT('Ctrl Pts',(0.0181151770099195,-0.205334791173908,
1.58121615104249));
#8390=CARTESIAN_POINT('Ctrl Pts',(-0.0448478169351064,-0.190512949205082,
1.57751124674856));
#8391=CARTESIAN_POINT('Ctrl Pts',(-0.107810810880132,-0.175691107236256,
1.57380634245464));
#8392=CARTESIAN_POINT('Ctrl Pts',(-0.162699153184846,-0.126568249010039,
1.57010143816071));
#8393=CARTESIAN_POINT('Ctrl Pts',(-0.184389058707223,-0.0656291515085119,
1.56639653386679));
#8394=CARTESIAN_POINT('Ctrl Pts',(-0.191823267607932,-0.0447422933071413,
1.565126678982));
#8395=CARTESIAN_POINT('Ctrl Pts',(-0.195357411599742,-0.0224672944395423,
1.56385682409721));
#8396=CARTESIAN_POINT('Ctrl Pts',(-0.195203598247727,-0.000145069483009505,
1.56258696921242));
#8397=CARTESIAN_POINT('Ctrl Pts',(-0.195226188848194,-0.00015379427405286,
1.55241303078758));
#8398=CARTESIAN_POINT('Ctrl Pts',(-0.195383489323086,-0.0215159109049027,
1.55362862167461));
#8399=CARTESIAN_POINT('Ctrl Pts',(-0.192151945114518,-0.0428317550682234,
1.55484421256164));
#8400=CARTESIAN_POINT('Ctrl Pts',(-0.185328327706693,-0.0629279169161807,
1.55605980344866));
#8401=CARTESIAN_POINT('Ctrl Pts',(-0.164531158441829,-0.124177435250376,
1.55976470774259));
#8402=CARTESIAN_POINT('Ctrl Pts',(-0.110366441153868,-0.174097059683963,
1.56346961203652));
#8403=CARTESIAN_POINT('Ctrl Pts',(-0.0476267394780286,-0.189837313151712,
1.56717451633044));
#8404=CARTESIAN_POINT('Ctrl Pts',(0.0151129621978108,-0.205577566619462,
1.57087942062437));
#8405=CARTESIAN_POINT('Ctrl Pts',(0.0864276482615303,-0.187138449121373,
1.57458432491829));
#8406=CARTESIAN_POINT('Ctrl Pts',(0.133674779789486,-0.142960011983078,
1.57828922921222));
#8407=CARTESIAN_POINT('Ctrl Pts',(0.180921911317442,-0.0987815748447818,
1.58199413350614));
#8408=CARTESIAN_POINT('Ctrl Pts',(0.204101488309635,-0.0288638180662828,
1.58569903780007));
#8409=CARTESIAN_POINT('Ctrl Pts',(0.192603631006867,0.0347901293607817,
1.58940394209399));
#8410=CARTESIAN_POINT('Ctrl Pts',(0.181105773704099,0.0984440767878479,
1.59310884638792));
#8411=CARTESIAN_POINT('Ctrl Pts',(0.134930482106364,0.155834214863477,1.59681375068184));
#8412=CARTESIAN_POINT('Ctrl Pts',(0.0752133572586277,0.180691623125853,
1.60051865497577));
#8413=CARTESIAN_POINT('Ctrl Pts',(0.0154962324108934,0.205549031388229,
1.60422355926969));
#8414=CARTESIAN_POINT('Ctrl Pts',(-0.0577627256868428,0.197873709837356,
1.60792846356362));
#8415=CARTESIAN_POINT('Ctrl Pts',(-0.111031035533165,0.161178847639516,
1.61163336785754));
#8416=CARTESIAN_POINT('Ctrl Pts',(-0.162693586883228,0.125590141933467,
1.61522658883422));
#8417=CARTESIAN_POINT('Ctrl Pts',(-0.195552549538933,0.0627050974813158,
1.6188198098109));
#8418=CARTESIAN_POINT('Ctrl Pts',(-0.195712283470102,-3.61459064724743E-5,
1.62241303078758));
#8419=CARTESIAN_POINT('Origin',(0.,0.,0.));
#8420=CARTESIAN_POINT('',(-0.19536023340508,0.000178280042280071,1.70258696921242));
#8421=CARTESIAN_POINT('',(-0.195332200326426,0.000176344485861957,1.69241303078758));
#8422=CARTESIAN_POINT('',(-0.1954,-2.39295984553393E-17,0.));
#8423=CARTESIAN_POINT('Ctrl Pts',(-0.19536023340508,0.000178280042280071,
1.70258696921242));
#8424=CARTESIAN_POINT('Ctrl Pts',(-0.19550841731601,0.016632826172098,1.70164900895765));
#8425=CARTESIAN_POINT('Ctrl Pts',(-0.193603054742847,0.0330535488509283,
1.70071104870287));
#8426=CARTESIAN_POINT('Ctrl Pts',(-0.189510780251034,0.0489098626792897,
1.6997730884481));
#8427=CARTESIAN_POINT('Ctrl Pts',(-0.17334646490881,0.11154164786371,1.69606818415418));
#8428=CARTESIAN_POINT('Ctrl Pts',(-0.123061569409359,0.165367427987009,
1.69236327986025));
#8429=CARTESIAN_POINT('Ctrl Pts',(-0.0616727646407164,0.185749779542894,
1.68865837556633));
#8430=CARTESIAN_POINT('Ctrl Pts',(-0.000283959872074024,0.206132131098779,
1.6849534712724));
#8431=CARTESIAN_POINT('Ctrl Pts',(0.0722087541657616,0.193071054087249,
1.68124856697847));
#8432=CARTESIAN_POINT('Ctrl Pts',(0.122623625294196,0.152544934423833,1.67754366268455));
#8433=CARTESIAN_POINT('Ctrl Pts',(0.173038496422631,0.112018814760415,1.67383875839062));
#8434=CARTESIAN_POINT('Ctrl Pts',(0.201375524641664,0.0440276524451133,
1.6701338540967));
#8435=CARTESIAN_POINT('Ctrl Pts',(0.194664134075893,-0.0203072746360924,
1.66642894980277));
#8436=CARTESIAN_POINT('Ctrl Pts',(0.187952743510121,-0.0846422017172963,
1.66272404550885));
#8437=CARTESIAN_POINT('Ctrl Pts',(0.146192934159544,-0.145320893564402,
1.65901914121492));
#8438=CARTESIAN_POINT('Ctrl Pts',(0.088499228956397,-0.174569175322524,
1.655314236921));
#8439=CARTESIAN_POINT('Ctrl Pts',(0.0308055237532497,-0.203817457080646,
1.65160933262707));
#8440=CARTESIAN_POINT('Ctrl Pts',(-0.0428220773024696,-0.201635328749786,
1.64790442833315));
#8441=CARTESIAN_POINT('Ctrl Pts',(-0.0986823554860735,-0.169021605762054,
1.64419952403922));
#8442=CARTESIAN_POINT('Ctrl Pts',(-0.154542633669677,-0.136407882774321,
1.64049461974529));
#8443=CARTESIAN_POINT('Ctrl Pts',(-0.192635588981168,-0.0733625651297149,
1.63678971545137));
#8444=CARTESIAN_POINT('Ctrl Pts',(-0.195525110499984,-0.00874309228087092,
1.63308481115744));
#8445=CARTESIAN_POINT('Ctrl Pts',(-0.195654535796742,-0.00584870495917813,
1.63291886384244));
#8446=CARTESIAN_POINT('Ctrl Pts',(-0.195713333973045,-0.00295115947825913,
1.63275291652743));
#8447=CARTESIAN_POINT('Ctrl Pts',(-0.195702834179537,-5.31785447526745E-5,
1.63258696921242));
#8448=CARTESIAN_POINT('Ctrl Pts',(-0.195712283470102,-3.61459064724743E-5,
1.62241303078758));
#8449=CARTESIAN_POINT('Ctrl Pts',(-0.195717248267821,-0.00198624867923799,
1.62252471410483));
#8450=CARTESIAN_POINT('Ctrl Pts',(-0.195690623309908,-0.0039362125300576,
1.62263639742207));
#8451=CARTESIAN_POINT('Ctrl Pts',(-0.195631991350833,-0.00588521351159191,
1.62274808073932));
#8452=CARTESIAN_POINT('Ctrl Pts',(-0.193686975727267,-0.0705400096200497,
1.62645298503325));
#8453=CARTESIAN_POINT('Ctrl Pts',(-0.156519282885226,-0.134135198992158,
1.63015788932717));
#8454=CARTESIAN_POINT('Ctrl Pts',(-0.101141507666876,-0.167561651951873,
1.6338627936211));
#8455=CARTESIAN_POINT('Ctrl Pts',(-0.0457637324485236,-0.200988104911589,
1.63756769791502));
#8456=CARTESIAN_POINT('Ctrl Pts',(0.0278241251461387,-0.204245821458907,
1.64127260220895));
#8457=CARTESIAN_POINT('Ctrl Pts',(0.0859390379816513,-0.175843662179669,
1.64497750650287));
#8458=CARTESIAN_POINT('Ctrl Pts',(0.144053950817164,-0.147441502900431,
1.6486824107968));
#8459=CARTESIAN_POINT('Ctrl Pts',(0.186695918893525,-0.0873794677946378,
1.65238731509072));
#8460=CARTESIAN_POINT('Ctrl Pts',(0.19434663287583,-0.0231494723006056,
1.65609221938465));
#8461=CARTESIAN_POINT('Ctrl Pts',(0.201997346858136,0.0410805231934266,
1.65979712367858));
#8462=CARTESIAN_POINT('Ctrl Pts',(0.174656806746383,0.1094784790757,1.6635020279725));
#8463=CARTESIAN_POINT('Ctrl Pts',(0.124839470558294,0.15073691773648,1.66720693226643));
#8464=CARTESIAN_POINT('Ctrl Pts',(0.0750221343702045,0.19199535639726,1.67091183656035));
#8465=CARTESIAN_POINT('Ctrl Pts',(0.00272800210577999,0.20611427783655,
1.67461674085428));
#8466=CARTESIAN_POINT('Ctrl Pts',(-0.058952069966136,0.186631093938489,
1.6783216451482));
#8467=CARTESIAN_POINT('Ctrl Pts',(-0.120632142038052,0.167147910040428,
1.68202654944213));
#8468=CARTESIAN_POINT('Ctrl Pts',(-0.171698153917458,0.114062620805016,
1.68573145373605));
#8469=CARTESIAN_POINT('Ctrl Pts',(-0.188775897955746,0.0516737082951384,
1.68943635802998));
#8470=CARTESIAN_POINT('Ctrl Pts',(-0.193349552352469,0.0349651006846826,
1.69042858228251));
#8471=CARTESIAN_POINT('Ctrl Pts',(-0.19548542556344,0.0175891981745919,
1.69142080653505));
#8472=CARTESIAN_POINT('Ctrl Pts',(-0.195332200326426,0.000176344485861957,
1.69241303078758));
#8473=CARTESIAN_POINT('Origin',(0.,0.,0.));
#8474=CARTESIAN_POINT('',(-0.195093080635393,-5.39352580709168E-5,1.77258696921242));
#8475=CARTESIAN_POINT('',(-0.1951020484266,-6.86943200097011E-5,1.76241303078758));
#8476=CARTESIAN_POINT('',(-0.1954,-2.39295984553393E-17,0.));
#8477=CARTESIAN_POINT('Ctrl Pts',(-0.195093080635393,-5.39352580709168E-5,
1.77258696921242));
#8478=CARTESIAN_POINT('Ctrl Pts',(-0.195004235779033,0.0358901483346491,
1.77054510138787));
#8479=CARTESIAN_POINT('Ctrl Pts',(-0.185501828716737,0.0718779233040721,
1.76850323356331));
#8480=CARTESIAN_POINT('Ctrl Pts',(-0.166873611769098,0.102272714806047,
1.76646136573876));
#8481=CARTESIAN_POINT('Ctrl Pts',(-0.133073303968799,0.157423098290437,
1.76275646144483));
#8482=CARTESIAN_POINT('Ctrl Pts',(-0.0692281383564483,0.194159730542236,
1.75905155715091));
#8483=CARTESIAN_POINT('Ctrl Pts',(-0.0045616650676435,0.195667324074495,
1.75534665285698));
#8484=CARTESIAN_POINT('Ctrl Pts',(0.0601048082211613,0.197174917606755,
1.75164174856306));
#8485=CARTESIAN_POINT('Ctrl Pts',(0.12559258918642,0.163453472419475,1.74793684426913));
#8486=CARTESIAN_POINT('Ctrl Pts',(0.161926261021679,0.109938148475413,1.74423193997521));
#8487=CARTESIAN_POINT('Ctrl Pts',(0.198259932856938,0.0564228245313505,
1.74052703568128));
#8488=CARTESIAN_POINT('Ctrl Pts',(0.205439495562197,-0.0168863781694949,
1.73682213138736));
#8489=CARTESIAN_POINT('Ctrl Pts',(0.180178681357328,-0.0764339798976696,
1.73311722709343));
#8490=CARTESIAN_POINT('Ctrl Pts',(0.154917867152459,-0.135981581625844,
1.7294123227995));
#8491=CARTESIAN_POINT('Ctrl Pts',(0.097216676037462,-0.181767582381348,
1.72570741850558));
#8492=CARTESIAN_POINT('Ctrl Pts',(0.0334864053323433,-0.192834569402327,
1.72200251421165));
#8493=CARTESIAN_POINT('Ctrl Pts',(-0.0302438653727754,-0.203901556423306,
1.71829760991773));
#8494=CARTESIAN_POINT('Ctrl Pts',(-0.100003215668016,-0.180249529709759,
1.7145927056238));
#8495=CARTESIAN_POINT('Ctrl Pts',(-0.143861023223137,-0.132704621230215,
1.71088780132988));
#8496=CARTESIAN_POINT('Ctrl Pts',(-0.176615472341799,-0.097196524212656,
1.70812085729073));
#8497=CARTESIAN_POINT('Ctrl Pts',(-0.194923096983834,-0.0483619519122345,
1.70535391325157));
#8498=CARTESIAN_POINT('Ctrl Pts',(-0.19536023340508,0.000178280042280071,
1.70258696921242));
#8499=CARTESIAN_POINT('Ctrl Pts',(-0.195332200326426,0.000176344485861957,
1.69241303078758));
#8500=CARTESIAN_POINT('Ctrl Pts',(-0.194913291958459,-0.0474293258497361,
1.69512571082897));
#8501=CARTESIAN_POINT('Ctrl Pts',(-0.177384701551267,-0.0953111847948915,
1.69783839087036));
#8502=CARTESIAN_POINT('Ctrl Pts',(-0.14578470180404,-0.130588408742416,
1.70055107091176));
#8503=CARTESIAN_POINT('Ctrl Pts',(-0.102626285416879,-0.178769077485746,
1.70425597520568));
#8504=CARTESIAN_POINT('Ctrl Pts',(-0.0332199764453863,-0.203437879188069,
1.70796087949961));
#8505=CARTESIAN_POINT('Ctrl Pts',(0.030665198740133,-0.193303278203442,
1.71166578379353));
#8506=CARTESIAN_POINT('Ctrl Pts',(0.0945503739256559,-0.183168677218815,
1.71537068808746));
#8507=CARTESIAN_POINT('Ctrl Pts',(0.152914415325207,-0.138230673547234,
1.71907559238138));
#8508=CARTESIAN_POINT('Ctrl Pts',(0.179042622246928,-0.0790585301970201,
1.72278049667531));
#8509=CARTESIAN_POINT('Ctrl Pts',(0.205170829168648,-0.0198863868468077,
1.72648540096923));
#8510=CARTESIAN_POINT('Ctrl Pts',(0.199063201612543,0.053519896182033,1.73019030526316));
#8511=CARTESIAN_POINT('Ctrl Pts',(0.163515355478164,0.107560403033919,1.73389520955708));
#8512=CARTESIAN_POINT('Ctrl Pts',(0.127967509343785,0.161600909885804,1.73760011385101));
#8513=CARTESIAN_POINT('Ctrl Pts',(0.0629794446311314,0.196275640560732,
1.74130501814494));
#8514=CARTESIAN_POINT('Ctrl Pts',(-0.00170215464495672,0.195713092172021,
1.74500992243886));
#8515=CARTESIAN_POINT('Ctrl Pts',(-0.0663837539210485,0.19515054378331,
1.74871482673279));
#8516=CARTESIAN_POINT('Ctrl Pts',(-0.130758887760577,0.159350716330956,
1.75241973102671));
#8517=CARTESIAN_POINT('Ctrl Pts',(-0.165361426140981,0.104700098006593,
1.75612463532064));
#8518=CARTESIAN_POINT('Ctrl Pts',(-0.184938580117925,0.0737802979009116,
1.75822076714295));
#8519=CARTESIAN_POINT('Ctrl Pts',(-0.194985580686779,0.0368263940799281,
1.76031689896526));
#8520=CARTESIAN_POINT('Ctrl Pts',(-0.1951020484266,-6.86943200097011E-5,
1.76241303078758));
#8521=CARTESIAN_POINT('Origin',(0.,0.,0.));
#8522=CARTESIAN_POINT('',(-0.195557989435191,-0.000150381408634326,1.84258696921242));
#8523=CARTESIAN_POINT('',(-0.195583821122648,-0.000140590296505579,1.83241303078758));
#8524=CARTESIAN_POINT('',(-0.1954,-2.39295984553393E-17,0.));
#8525=CARTESIAN_POINT('Ctrl Pts',(-0.195557989435191,-0.000150381408634326,
1.84258696921242));
#8526=CARTESIAN_POINT('Ctrl Pts',(-0.195089679602252,0.054892193728964,
1.83944119381809));
#8527=CARTESIAN_POINT('Ctrl Pts',(-0.170755613617913,0.110297227528981,
1.83629541842375));
#8528=CARTESIAN_POINT('Ctrl Pts',(-0.129599212359622,0.14666476964298,1.83314964302941));
#8529=CARTESIAN_POINT('Ctrl Pts',(-0.0811276882899435,0.189496264599762,
1.82944473873549));
#8530=CARTESIAN_POINT('Ctrl Pts',(-0.00932239762518191,0.205921414639302,
1.82573983444156));
#8531=CARTESIAN_POINT('Ctrl Pts',(0.0529495585532175,0.18842201237563,1.82203493014764));
#8532=CARTESIAN_POINT('Ctrl Pts',(0.115221514731615,0.17092261011196,1.81833002585371));
#8533=CARTESIAN_POINT('Ctrl Pts',(0.167960136423649,0.119498655545081,1.81462512155979));
#8534=CARTESIAN_POINT('Ctrl Pts',(0.187025620085586,0.0576881957619144,
1.81092021726586));
#8535=CARTESIAN_POINT('Ctrl Pts',(0.206091103747522,-0.00412226402125245,
1.80721531297194));
#8536=CARTESIAN_POINT('Ctrl Pts',(0.191483449379358,-0.0763192290207106,
1.80351040867801));
#8537=CARTESIAN_POINT('Ctrl Pts',(0.149888950542983,-0.125856318887,1.79980550438409));
#8538=CARTESIAN_POINT('Ctrl Pts',(0.108294451706606,-0.17539340875329,1.79610060009016));
#8539=CARTESIAN_POINT('Ctrl Pts',(0.0397131084020174,-0.202270623486414,
1.79239569579624));
#8540=CARTESIAN_POINT('Ctrl Pts',(-0.0244636606908309,-0.194185580835104,
1.78869079150231));
#8541=CARTESIAN_POINT('Ctrl Pts',(-0.0886404297836792,-0.186100538183794,
1.78498588720838));
#8542=CARTESIAN_POINT('Ctrl Pts',(-0.148412624664785,-0.14305323814805,
1.78128098291446));
#8543=CARTESIAN_POINT('Ctrl Pts',(-0.176420997111215,-0.0847475207716867,
1.77757607862053));
#8544=CARTESIAN_POINT('Ctrl Pts',(-0.188993236805098,-0.0585755803713125,
1.77591304215116));
#8545=CARTESIAN_POINT('Ctrl Pts',(-0.195165441948141,-0.0293292493376349,
1.77425000568179));
#8546=CARTESIAN_POINT('Ctrl Pts',(-0.195093080635393,-5.39352580709168E-5,
1.77258696921242));
#8547=CARTESIAN_POINT('Ctrl Pts',(-0.1951020484266,-6.86943200097011E-5,
1.76241303078758));
#8548=CARTESIAN_POINT('Ctrl Pts',(-0.195191436933401,-0.0283855214983397,
1.76402180325919));
#8549=CARTESIAN_POINT('Ctrl Pts',(-0.189431246293547,-0.0566677034601064,
1.7656305757308));
#8550=CARTESIAN_POINT('Ctrl Pts',(-0.177640467639129,-0.0821606720695544,
1.76723934820241));
#8551=CARTESIAN_POINT('Ctrl Pts',(-0.150487027835591,-0.14086941462497,
1.77094425249634));
#8552=CARTESIAN_POINT('Ctrl Pts',(-0.0913502053072345,-0.18478549053943,
1.77464915679026));
#8553=CARTESIAN_POINT('Ctrl Pts',(-0.0272984222508209,-0.193807399034674,
1.77835406108419));
#8554=CARTESIAN_POINT('Ctrl Pts',(0.0367533608055927,-0.202829307529917,
1.78205896537811));
#8555=CARTESIAN_POINT('Ctrl Pts',(0.105720104390061,-0.176957048605944,
1.78576386967204));
#8556=CARTESIAN_POINT('Ctrl Pts',(0.148033982348499,-0.128033010774619,
1.78946877396596));
#8557=CARTESIAN_POINT('Ctrl Pts',(0.190347860306936,-0.0791089729432942,
1.79317367825989));
#8558=CARTESIAN_POINT('Ctrl Pts',(0.206008872639341,-0.00713315620461422,
1.79687858255381));
#8559=CARTESIAN_POINT('Ctrl Pts',(0.187848577151528,0.0549492842548083,
1.80058348684774));
#8560=CARTESIAN_POINT('Ctrl Pts',(0.169688281663715,0.117031724714231,1.80428839114167));
#8561=CARTESIAN_POINT('Ctrl Pts',(0.117706678355686,0.169220788894399,1.80799329543559));
#8562=CARTESIAN_POINT('Ctrl Pts',(0.0556970642739923,0.187628219650532,
1.81169819972952));
#8563=CARTESIAN_POINT('Ctrl Pts',(-0.00631254980769992,0.206035650406663,
1.81540310402344));
#8564=CARTESIAN_POINT('Ctrl Pts',(-0.0783501746630549,0.190661447738761,
1.81910800831737));
#8565=CARTESIAN_POINT('Ctrl Pts',(-0.127442363964252,0.148542773789816,
1.82281291261129));
#8566=CARTESIAN_POINT('Ctrl Pts',(-0.169844792514325,0.112163584184181,
1.82601295200339));
#8567=CARTESIAN_POINT('Ctrl Pts',(-0.195129223210545,0.0558321996894708,
1.82921299139548));
#8568=CARTESIAN_POINT('Ctrl Pts',(-0.195583821122648,-0.000140590296505579,
1.83241303078758));
#8569=CARTESIAN_POINT('Origin',(0.,0.,0.));
#8570=CARTESIAN_POINT('',(-0.195564939510846,0.000147924627282119,1.91258696921242));
#8571=CARTESIAN_POINT('',(-0.195538264906755,0.000156701382499669,1.90241303078758));
#8572=CARTESIAN_POINT('',(-0.1954,-2.39295984553393E-17,0.));
#8573=CARTESIAN_POINT('Ctrl Pts',(-0.195564939510846,0.000147924627282119,
1.91258696921242));
#8574=CARTESIAN_POINT('Ctrl Pts',(-0.195645138896524,0.00967919899870748,
1.91204219054223));
#8575=CARTESIAN_POINT('Ctrl Pts',(-0.195008580056017,0.0191997185565135,
1.91149741187204));
#8576=CARTESIAN_POINT('Ctrl Pts',(-0.193618292474229,0.0286088678214767,
1.91095263320185));
#8577=CARTESIAN_POINT('Ctrl Pts',(-0.184163292281677,0.0925981526840929,
1.90724772890792));
#8578=CARTESIAN_POINT('Ctrl Pts',(-0.139848172472072,0.151436537073306,
1.903542824614));
#8579=CARTESIAN_POINT('Ctrl Pts',(-0.0809570863262455,0.178192201491052,
1.89983792032007));
#8580=CARTESIAN_POINT('Ctrl Pts',(-0.0220660001804177,0.204947865908799,
1.89613301602615));
#8581=CARTESIAN_POINT('Ctrl Pts',(0.0514010523016335,0.199620810355078,
1.89242811173222));
#8582=CARTESIAN_POINT('Ctrl Pts',(0.105816339545683,0.164649363144276,1.8887232074383));
#8583=CARTESIAN_POINT('Ctrl Pts',(0.16023162678973,0.129677915933475,1.88501830314437));
#8584=CARTESIAN_POINT('Ctrl Pts',(0.19559514879578,0.0650620770655954,1.88131339885044));
#8585=CARTESIAN_POINT('Ctrl Pts',(0.195720125430942,0.000378153354130759,
1.87760849455652));
#8586=CARTESIAN_POINT('Ctrl Pts',(0.195845102066104,-0.0643057703573357,
1.87390359026259));
#8587=CARTESIAN_POINT('Ctrl Pts',(0.160731533330379,-0.129057778912385,
1.87019868596867));
#8588=CARTESIAN_POINT('Ctrl Pts',(0.106451789411018,-0.164239237181177,
1.86649378167474));
#8589=CARTESIAN_POINT('Ctrl Pts',(0.0521720454916558,-0.199420695449971,
1.86278887738082));
#8590=CARTESIAN_POINT('Ctrl Pts',(-0.0212738736113445,-0.2050316034325,
1.85908397308689));
#8591=CARTESIAN_POINT('Ctrl Pts',(-0.080267909606869,-0.1785037063649,1.85537906879297));
#8592=CARTESIAN_POINT('Ctrl Pts',(-0.139261945602394,-0.1519758092973,1.85167416449904));
#8593=CARTESIAN_POINT('Ctrl Pts',(-0.183804098490444,-0.0933091071795703,
1.84796926020512));
#8594=CARTESIAN_POINT('Ctrl Pts',(-0.193506296197169,-0.0293568361836938,
1.84426435591119));
#8595=CARTESIAN_POINT('Ctrl Pts',(-0.194970511922324,-0.0197054227944751,
1.8437052270116));
#8596=CARTESIAN_POINT('Ctrl Pts',(-0.195641226643426,-0.00993362738438461,
1.84314609811201));
#8597=CARTESIAN_POINT('Ctrl Pts',(-0.195557989435191,-0.000150381408634326,
1.84258696921242));
#8598=CARTESIAN_POINT('Ctrl Pts',(-0.195583821122648,-0.000140590296505579,
1.83241303078758));
#8599=CARTESIAN_POINT('Ctrl Pts',(-0.195655542280467,-0.0089713244403536,
1.83291789568941));
#8600=CARTESIAN_POINT('Ctrl Pts',(-0.195109227819557,-0.0177931328624295,
1.83342276059124));
#8601=CARTESIAN_POINT('Ctrl Pts',(-0.193914593457294,-0.0265262553380925,
1.83392762549307));
#8602=CARTESIAN_POINT('Ctrl Pts',(-0.185147879902098,-0.0906134652870637,
1.837632529787));
#8603=CARTESIAN_POINT('Ctrl Pts',(-0.141467699044668,-0.149924739955016,
1.84133743408092));
#8604=CARTESIAN_POINT('Ctrl Pts',(-0.0828675765180874,-0.177311805980279,
1.84504233837484));
#8605=CARTESIAN_POINT('Ctrl Pts',(-0.0242674539915072,-0.204698872005543,
1.84874724266877));
#8606=CARTESIAN_POINT('Ctrl Pts',(0.0492526102042225,-0.200161729388119,
1.8524521469627));
#8607=CARTESIAN_POINT('Ctrl Pts',(0.104040619690215,-0.165777143275077,
1.85615705125662));
#8608=CARTESIAN_POINT('Ctrl Pts',(0.158828629176207,-0.131392557162035,
1.85986195555055));
#8609=CARTESIAN_POINT('Ctrl Pts',(0.194884583952461,-0.0671605275533752,
1.86356685984447));
#8610=CARTESIAN_POINT('Ctrl Pts',(0.195704759860937,-0.00248168203892953,
1.8672717641384));
#8611=CARTESIAN_POINT('Ctrl Pts',(0.196524935769412,0.062197163475518,1.87097666843232));
#8612=CARTESIAN_POINT('Ctrl Pts',(0.162109332810106,0.127322824895751,1.87468157272625));
#8613=CARTESIAN_POINT('Ctrl Pts',(0.108210844547972,0.163085636707173,1.87838647702018));
#8614=CARTESIAN_POINT('Ctrl Pts',(0.0543123562858388,0.198848448518593,
1.8820913813141));
#8615=CARTESIAN_POINT('Ctrl Pts',(-0.0190690172791211,0.205248410721205,
1.88579628560802));
#8616=CARTESIAN_POINT('Ctrl Pts',(-0.0783447619841414,0.179356098439996,
1.88950118990195));
#8617=CARTESIAN_POINT('Ctrl Pts',(-0.13762050668916,0.153463786158788,1.89320609419588));
#8618=CARTESIAN_POINT('Ctrl Pts',(-0.18279062253424,0.0952791993937629,
1.8969109984898));
#8619=CARTESIAN_POINT('Ctrl Pts',(-0.193179602887536,0.031434897903176,
1.90061590278373));
#8620=CARTESIAN_POINT('Ctrl Pts',(-0.194859387846714,0.0211119697883842,
1.90121494545168));
#8621=CARTESIAN_POINT('Ctrl Pts',(-0.195629876801359,0.0106410776720159,
1.90181398811963));
#8622=CARTESIAN_POINT('Ctrl Pts',(-0.195538264906755,0.000156701382499669,
1.90241303078758));
#8623=CARTESIAN_POINT('Origin',(0.,0.,0.));
#8624=CARTESIAN_POINT('',(-0.195095239123403,5.78821923055833E-5,1.98258696921242));
#8625=CARTESIAN_POINT('',(-0.195087892673083,4.28153426326047E-5,1.97241303078758));
#8626=CARTESIAN_POINT('',(-0.1954,-2.39295984553393E-17,0.));
#8627=CARTESIAN_POINT('Ctrl Pts',(-0.195095239123403,5.78821923055833E-5,
1.98258696921242));
#8628=CARTESIAN_POINT('Ctrl Pts',(-0.19517227391142,0.0290797798957806,
1.98093828297245));
#8629=CARTESIAN_POINT('Ctrl Pts',(-0.189110562653447,0.0580710867028783,
1.97928959673248));
#8630=CARTESIAN_POINT('Ctrl Pts',(-0.176747162247964,0.0840651600602401,
1.97764091049251));
#8631=CARTESIAN_POINT('Ctrl Pts',(-0.148964304516005,0.14247867238501,1.97393600619858));
#8632=CARTESIAN_POINT('Ctrl Pts',(-0.0893588997550408,0.185756623405738,
1.97023110190465));
#8633=CARTESIAN_POINT('Ctrl Pts',(-0.0252138521235489,0.1940895982781,1.96652619761073));
#8634=CARTESIAN_POINT('Ctrl Pts',(0.0389311955079449,0.202422573150462,
1.9628212933168));
#8635=CARTESIAN_POINT('Ctrl Pts',(0.107615886009967,0.175810571874455,1.95911638902288));
#8636=CARTESIAN_POINT('Ctrl Pts',(0.149401496071477,0.12643458178152,1.95541148472895));
#8637=CARTESIAN_POINT('Ctrl Pts',(0.191187106132985,0.0770585916885855,
1.95170658043503));
#8638=CARTESIAN_POINT('Ctrl Pts',(0.206073635753984,0.00491861277872399,
1.9480016761411));
#8639=CARTESIAN_POINT('Ctrl Pts',(0.187247143102674,-0.0569650585758442,
1.94429677184718));
#8640=CARTESIAN_POINT('Ctrl Pts',(0.168420650451363,-0.118848729930418,
1.94059186755325));
#8641=CARTESIAN_POINT('Ctrl Pts',(0.115881135527736,-0.170476093729696,
1.93688696325933));
#8642=CARTESIAN_POINT('Ctrl Pts',(0.0536772656622717,-0.188215997326701,
1.9331820589654));
#8643=CARTESIAN_POINT('Ctrl Pts',(-0.00852660420318736,-0.205955900923705,
1.92947715467148));
#8644=CARTESIAN_POINT('Ctrl Pts',(-0.0803948290104825,-0.189808344318442,
1.92577225037755));
#8645=CARTESIAN_POINT('Ctrl Pts',(-0.129031501126381,-0.147164473347801,
1.92206734608362));
#8646=CARTESIAN_POINT('Ctrl Pts',(-0.170516511699694,-0.110791067003543,
1.91890722045989));
#8647=CARTESIAN_POINT('Ctrl Pts',(-0.195099722813576,-0.0551406283503992,
1.91574709483616));
#8648=CARTESIAN_POINT('Ctrl Pts',(-0.195564939510846,0.000147924627282119,
1.91258696921242));
#8649=CARTESIAN_POINT('Ctrl Pts',(-0.195538264906755,0.000156701382499669,
1.90241303078758));
#8650=CARTESIAN_POINT('Ctrl Pts',(-0.195063283936023,-0.0542017337207628,
1.90551889241355));
#8651=CARTESIAN_POINT('Ctrl Pts',(-0.171413995491211,-0.108922639612492,
1.90862475403953));
#8652=CARTESIAN_POINT('Ctrl Pts',(-0.131168044975528,-0.145263401293193,
1.9117306156655));
#8653=CARTESIAN_POINT('Ctrl Pts',(-0.0831596618487121,-0.188613382782822,
1.91543551995943));
#8654=CARTESIAN_POINT('Ctrl Pts',(-0.0115350507335688,-0.205809329545931,
1.91914042425335));
#8655=CARTESIAN_POINT('Ctrl Pts',(0.0509213888967292,-0.188980221004203,
1.92284532854728));
#8656=CARTESIAN_POINT('Ctrl Pts',(0.113377828527027,-0.172151112462475,
1.9265502328412));
#8657=CARTESIAN_POINT('Ctrl Pts',(0.166666096672482,-0.12129694861591,1.93025513713513));
#8658=CARTESIAN_POINT('Ctrl Pts',(0.186394802679598,-0.0596949689002616,
1.93396004142905));
#8659=CARTESIAN_POINT('Ctrl Pts',(0.206123508686714,0.00190701081538635,
1.93766494572298));
#8660=CARTESIAN_POINT('Ctrl Pts',(0.192292652555493,0.0742568064001138,
1.94136985001691));
#8661=CARTESIAN_POINT('Ctrl Pts',(0.151232967610728,0.124238083072873,1.94507475431083));
#8662=CARTESIAN_POINT('Ctrl Pts',(0.11017328266596,0.174219359745633,1.94877965860476));
#8663=CARTESIAN_POINT('Ctrl Pts',(0.041884768907644,0.201832117506419,1.95248456289868));
#8664=CARTESIAN_POINT('Ctrl Pts',(-0.0223751904878854,0.19443729742156,
1.95618946719261));
#8665=CARTESIAN_POINT('Ctrl Pts',(-0.086635149883413,0.187042477336701,
1.95989437148653));
#8666=CARTESIAN_POINT('Ctrl Pts',(-0.146866554916156,0.144640079406198,
1.96359927578046));
#8667=CARTESIAN_POINT('Ctrl Pts',(-0.175499965240401,0.0866387556384964,
1.96730418007438));
#8668=CARTESIAN_POINT('Ctrl Pts',(-0.188661242577225,0.0599785883945253,
1.96900713031211));
#8669=CARTESIAN_POINT('Ctrl Pts',(-0.195146625645364,0.0300227443028642,
1.97071008054985));
#8670=CARTESIAN_POINT('Ctrl Pts',(-0.195087892673083,4.28153426326047E-5,
1.97241303078758));
#8671=CARTESIAN_POINT('Origin',(0.,0.,0.));
#8672=CARTESIAN_POINT('',(-0.195352761517788,-0.000177909769055379,2.05258696921242));
#8673=CARTESIAN_POINT('',(-0.195381194231368,-0.000178768183475579,2.04241303078758));
#8674=CARTESIAN_POINT('',(-0.1954,-2.39295984553393E-17,0.));
#8675=CARTESIAN_POINT('Ctrl Pts',(-0.195352761517788,-0.000177909769055379,
2.05258696921242));
#8676=CARTESIAN_POINT('Ctrl Pts',(-0.194920193265683,0.0481152823703308,
2.04983437540267));
#8677=CARTESIAN_POINT('Ctrl Pts',(-0.176820579764667,0.0966981301161916,
2.04708178159292));
#8678=CARTESIAN_POINT('Ctrl Pts',(-0.144372747816328,0.132147721079886,
2.04432918778316));
#8679=CARTESIAN_POINT('Ctrl Pts',(-0.100698991271494,0.179861750412485,
2.04062428348924));
#8680=CARTESIAN_POINT('Ctrl Pts',(-0.0310315582308591,0.20378316539473,
2.03691937919531));
#8681=CARTESIAN_POINT('Ctrl Pts',(0.0327410018324499,0.192962528221534,
2.03321447490139));
#8682=CARTESIAN_POINT('Ctrl Pts',(0.096513561895759,0.182141891048337,2.02950957060746));
#8683=CARTESIAN_POINT('Ctrl Pts',(0.154391248981745,0.136579201719707,2.02580466631354));
#8684=CARTESIAN_POINT('Ctrl Pts',(0.179881979091815,0.0771296576985378,
2.02209976201961));
#8685=CARTESIAN_POINT('Ctrl Pts',(0.205372709201885,0.0176801136773685,
2.01839485772569));
#8686=CARTESIAN_POINT('Ctrl Pts',(0.198476482336034,-0.055656285036337,
2.01468995343176));
#8687=CARTESIAN_POINT('Ctrl Pts',(0.162349876281112,-0.109311610408804,
2.01098504913783));
#8688=CARTESIAN_POINT('Ctrl Pts',(0.12622327022619,-0.162966935781272,2.00728014484391));
#8689=CARTESIAN_POINT('Ctrl Pts',(0.0608662849821969,-0.196941187812501,
2.00357524054998));
#8690=CARTESIAN_POINT('Ctrl Pts',(-0.0038055311604717,-0.195683490441188,
1.99987033625606));
#8691=CARTESIAN_POINT('Ctrl Pts',(-0.0684773473031403,-0.194425793069875,
1.99616543196213));
#8692=CARTESIAN_POINT('Ctrl Pts',(-0.132463994344484,-0.15793614629602,
1.99246052766821));
#8693=CARTESIAN_POINT('Ctrl Pts',(-0.16647716251368,-0.102916786094686,
1.98875562337428));
#8694=CARTESIAN_POINT('Ctrl Pts',(-0.185354435693536,-0.072381098047782,
1.98669940532033));
#8695=CARTESIAN_POINT('Ctrl Pts',(-0.194999162430299,-0.0361378162802388,
1.98464318726638));
#8696=CARTESIAN_POINT('Ctrl Pts',(-0.195095239123403,5.78821923055833E-5,
1.98258696921242));
#8697=CARTESIAN_POINT('Ctrl Pts',(-0.195087892673083,4.28153426326047E-5,
1.97241303078758));
#8698=CARTESIAN_POINT('Ctrl Pts',(-0.195018847371885,-0.0352009863002633,
1.97441498484377));
#8699=CARTESIAN_POINT('Ctrl Pts',(-0.18590591169575,-0.0704780729444801,
1.97641693889997));
#8700=CARTESIAN_POINT('Ctrl Pts',(-0.167963177482808,-0.100473293903646,
1.97841889295616));
#8701=CARTESIAN_POINT('Ctrl Pts',(-0.13475756378522,-0.155983770073185,
1.98212379725009));
#8702=CARTESIAN_POINT('Ctrl Pts',(-0.0713109207742939,-0.19340447280736,
1.98582870154401));
#8703=CARTESIAN_POINT('Ctrl Pts',(-0.00666438469241006,-0.195606998225116,
1.98953360583794));
#8704=CARTESIAN_POINT('Ctrl Pts',(0.0579821513894738,-0.197809523642872,
1.99323851013186));
#8705=CARTESIAN_POINT('Ctrl Pts',(0.123828580542316,-0.164793871744207,
1.99694341442579));
#8706=CARTESIAN_POINT('Ctrl Pts',(0.160735323596081,-0.111672143018891,
2.00064831871971));
#8707=CARTESIAN_POINT('Ctrl Pts',(0.197642066649846,-0.0585504142935751,
2.00435322301364));
#8708=CARTESIAN_POINT('Ctrl Pts',(0.205609123604535,0.0146773912583926,
2.00805812730756));
#8709=CARTESIAN_POINT('Ctrl Pts',(0.180989770606949,0.0744930514451918,
2.01176303160149));
#8710=CARTESIAN_POINT('Ctrl Pts',(0.156370417609364,0.134308711631991,2.01546793589541));
#8711=CARTESIAN_POINT('Ctrl Pts',(0.0991646546595033,0.180712226453622,
2.01917284018934));
#8712=CARTESIAN_POINT('Ctrl Pts',(0.0355570090520971,0.192463531312391,
2.02287774448326));
#8713=CARTESIAN_POINT('Ctrl Pts',(-0.0280506365553108,0.20421483617116,
2.02658264877719));
#8714=CARTESIAN_POINT('Ctrl Pts',(-0.098060164820265,0.181313931067065,
2.03028755307112));
#8715=CARTESIAN_POINT('Ctrl Pts',(-0.142426440616362,0.134243140574553,
2.03399245736504));
#8716=CARTESIAN_POINT('Ctrl Pts',(-0.176038598375119,0.0985820261926483,
2.03679931517255));
#8717=CARTESIAN_POINT('Ctrl Pts',(-0.194932378367354,0.0490481979593188,
2.03960617298007));
#8718=CARTESIAN_POINT('Ctrl Pts',(-0.195381194231368,-0.000178768183475579,
2.04241303078758));
#8719=CARTESIAN_POINT('Origin',(0.,0.,0.));
#8720=CARTESIAN_POINT('',(-0.195705652066383,4.87247307793624E-5,2.12258696921242));
#8721=CARTESIAN_POINT('',(-0.195693853754418,6.53393013630089E-5,2.11241303078758));
#8722=CARTESIAN_POINT('',(-0.1954,-2.39295984553393E-17,0.));
#8723=CARTESIAN_POINT('Ctrl Pts',(-0.195705652066383,4.87247307793624E-5,
2.12258696921242));
#8724=CARTESIAN_POINT('Ctrl Pts',(-0.195714515890613,0.0026960020070379,
2.12243537212681));
#8725=CARTESIAN_POINT('Ctrl Pts',(-0.195665450924563,0.0053429432466519,
2.12228377504121));
#8726=CARTESIAN_POINT('Ctrl Pts',(-0.195557435859476,0.00798747668964042,
2.1221321779556));
#8727=CARTESIAN_POINT('Ctrl Pts',(-0.192917639211396,0.07261763279738,2.11842727366167));
#8728=CARTESIAN_POINT('Ctrl Pts',(-0.155068588696691,0.1358096789777,2.11472236936775));
#8729=CARTESIAN_POINT('Ctrl Pts',(-0.0993347538758449,0.168639014380346,
2.11101746507382));
#8730=CARTESIAN_POINT('Ctrl Pts',(-0.0436009190549989,0.201468349782991,
2.10731256077989));
#8731=CARTESIAN_POINT('Ctrl Pts',(0.030017700071986,0.203934974407961,2.10360765648597));
#8732=CARTESIAN_POINT('Ctrl Pts',(0.0878239960609676,0.174909851675304,
2.09990275219204));
#8733=CARTESIAN_POINT('Ctrl Pts',(0.145630292049948,0.145884728942649,2.09619784789812));
#8734=CARTESIAN_POINT('Ctrl Pts',(0.187624264900923,0.0853678588523708,
2.09249294360419));
#8735=CARTESIAN_POINT('Ctrl Pts',(0.194584209101134,0.0210593463327518,
2.08878803931027));
#8736=CARTESIAN_POINT('Ctrl Pts',(0.201544153301344,-0.0432491661868709,
2.08508313501634));
#8737=CARTESIAN_POINT('Ctrl Pts',(0.173470068850782,-0.111349321135837,
2.08137823072242));
#8738=CARTESIAN_POINT('Ctrl Pts',(0.123212175605713,-0.15206995193368,2.07767332642849));
#8739=CARTESIAN_POINT('Ctrl Pts',(0.0729542823606449,-0.192790582731522,
2.07396842213457));
#8740=CARTESIAN_POINT('Ctrl Pts',(0.000512580321072716,-0.206131689378248,
2.07026351784064));
#8741=CARTESIAN_POINT('Ctrl Pts',(-0.0609545278221702,-0.18598670930055,
2.06655861354672));
#8742=CARTESIAN_POINT('Ctrl Pts',(-0.122421635965411,-0.165841729222853,
2.06285370925279));
#8743=CARTESIAN_POINT('Ctrl Pts',(-0.172914150212319,-0.112210662420741,
2.05914880495886));
#8744=CARTESIAN_POINT('Ctrl Pts',(-0.189320367311259,-0.0496418071782075,
2.05544390066494));
#8745=CARTESIAN_POINT('Ctrl Pts',(-0.193537429699225,-0.0335590768016581,
2.05449159018077));
#8746=CARTESIAN_POINT('Ctrl Pts',(-0.195502416465111,-0.0168858283241024,
2.05353927969659));
#8747=CARTESIAN_POINT('Ctrl Pts',(-0.195352761517788,-0.000177909769055379,
2.05258696921242));
#8748=CARTESIAN_POINT('Ctrl Pts',(-0.195381194231368,-0.000178768183475579,
2.04241303078758));
#8749=CARTESIAN_POINT('Ctrl Pts',(-0.195524791640772,-0.0159288014993712,
2.04331107727399));
#8750=CARTESIAN_POINT('Ctrl Pts',(-0.193780247164878,-0.0316474224925252,
2.0442091237604));
#8751=CARTESIAN_POINT('Ctrl Pts',(-0.19002550838013,-0.0468702244805944,
2.04510717024682));
#8752=CARTESIAN_POINT('Ctrl Pts',(-0.174535277020564,-0.10967212316231,
2.04881207454074));
#8753=CARTESIAN_POINT('Ctrl Pts',(-0.124831790974193,-0.164035244644817,
2.05251697883467));
#8754=CARTESIAN_POINT('Ctrl Pts',(-0.0636655952897654,-0.18507621066562,
2.05622188312859));
#8755=CARTESIAN_POINT('Ctrl Pts',(-0.00249939960533398,-0.206117176686425,
2.05992678742252));
#8756=CARTESIAN_POINT('Ctrl Pts',(0.0701295057171544,-0.193835987245522,
2.06363169171644));
#8757=CARTESIAN_POINT('Ctrl Pts',(0.120977030297591,-0.1538540539548,2.06733659601037));
#8758=CARTESIAN_POINT('Ctrl Pts',(0.171824554878027,-0.113872120664079,
2.0710415003043));
#8759=CARTESIAN_POINT('Ctrl Pts',(0.200890698716412,-0.0461894435235373,
2.07474640459822));
#8760=CARTESIAN_POINT('Ctrl Pts',(0.194871151241538,0.0182139010618868,
2.07845130889215));
#8761=CARTESIAN_POINT('Ctrl Pts',(0.188851603766663,0.082617245647309,2.08215621318607));
#8762=CARTESIAN_POINT('Ctrl Pts',(0.147746364978535,0.143741257677616,2.08586111748));
#8763=CARTESIAN_POINT('Ctrl Pts',(0.090370344278156,0.173607927966511,2.08956602177392));
#8764=CARTESIAN_POINT('Ctrl Pts',(0.0329943235777734,0.203474598255409,
2.09327092606785));
#8765=CARTESIAN_POINT('Ctrl Pts',(-0.0406524790348606,0.20208392680289,
2.09697583036177));
#8766=CARTESIAN_POINT('Ctrl Pts',(-0.0968600557997058,0.170072459170759,
2.1006807346557));
#8767=CARTESIAN_POINT('Ctrl Pts',(-0.153067632564546,0.138060991538631,
2.10438563894962));
#8768=CARTESIAN_POINT('Ctrl Pts',(-0.1918359834816,0.0754287277268964,2.10809054324355));
#8769=CARTESIAN_POINT('Ctrl Pts',(-0.195419851939884,0.0108440419851374,
2.11179544753747));
#8770=CARTESIAN_POINT('Ctrl Pts',(-0.195618987729891,0.00725542745666287,
2.11200130862084));
#8771=CARTESIAN_POINT('Ctrl Pts',(-0.195709494543343,0.00366078499822498,
2.11220716970421));
#8772=CARTESIAN_POINT('Ctrl Pts',(-0.195693853754418,6.53393013630089E-5,
2.11241303078758));
#8773=CARTESIAN_POINT('Origin',(0.,0.,0.));
#8774=CARTESIAN_POINT('',(-0.195209426648116,0.000147489598137318,2.19258696921242));
#8775=CARTESIAN_POINT('',(-0.19518796491764,0.000137929913403057,2.18241303078758));
#8776=CARTESIAN_POINT('',(-0.1954,-2.39295984553393E-17,0.));
#8777=CARTESIAN_POINT('Ctrl Pts',(-0.195209426648116,0.000147489598137318,
2.19258696921242));
#8778=CARTESIAN_POINT('Ctrl Pts',(-0.195364342248075,0.0222157994033578,
2.19133146455703));
#8779=CARTESIAN_POINT('Ctrl Pts',(-0.191911630624569,0.0442370720435746,
2.19007595990164));
#8780=CARTESIAN_POINT('Ctrl Pts',(-0.184641287577456,0.0649161428649712,
2.18882045524625));
#8781=CARTESIAN_POINT('Ctrl Pts',(-0.163187026091501,0.125938599413976,
2.18511555095233));
#8782=CARTESIAN_POINT('Ctrl Pts',(-0.108488913443121,0.175273191802267,
2.1814106466584));
#8783=CARTESIAN_POINT('Ctrl Pts',(-0.0455836640180361,0.190338225595007,
2.17770574236448));
#8784=CARTESIAN_POINT('Ctrl Pts',(0.0173215854070469,0.205403259387747,
2.17400083807055));
#8785=CARTESIAN_POINT('Ctrl Pts',(0.0884339716088341,0.186198734584936,
2.17029593377663));
#8786=CARTESIAN_POINT('Ctrl Pts',(0.135203554581594,0.141515049546657,2.1665910294827));
#8787=CARTESIAN_POINT('Ctrl Pts',(0.181973137554356,0.0968313645083757,
2.16288612518878));
#8788=CARTESIAN_POINT('Ctrl Pts',(0.204399917298089,0.026668519234623,2.15918122089485));
#8789=CARTESIAN_POINT('Ctrl Pts',(0.192218587828263,-0.0368581744443589,
2.15547631660092));
#8790=CARTESIAN_POINT('Ctrl Pts',(0.180037258358437,-0.100384868123344,
2.151771412307));
#8791=CARTESIAN_POINT('Ctrl Pts',(0.133247819675049,-0.157275410207558,
2.14806650801307));
#8792=CARTESIAN_POINT('Ctrl Pts',(0.073266983822997,-0.181489557782437,
2.14436160371915));
#8793=CARTESIAN_POINT('Ctrl Pts',(0.0132861479709503,-0.205703705357315,
2.14065669942522));
#8794=CARTESIAN_POINT('Ctrl Pts',(-0.059886085049757,-0.197241458422864,
2.1369517951313));
#8795=CARTESIAN_POINT('Ctrl Pts',(-0.112756930169383,-0.159976201938061,
2.13324689083737));
#8796=CARTESIAN_POINT('Ctrl Pts',(-0.163464408735403,-0.12423576332421,
2.12969358362906));
#8797=CARTESIAN_POINT('Ctrl Pts',(-0.195497891538502,-0.0620012110604251,
2.12614027642074));
#8798=CARTESIAN_POINT('Ctrl Pts',(-0.195705652066383,4.87247307793624E-5,
2.12258696921242));
#8799=CARTESIAN_POINT('Ctrl Pts',(-0.195693853754418,6.53393013630089E-5,
2.11241303078758));
#8800=CARTESIAN_POINT('Ctrl Pts',(-0.195428005564947,-0.0610468420235385,
2.11591207399813));
#8801=CARTESIAN_POINT('Ctrl Pts',(-0.164495934165812,-0.122391080297918,
2.11941111720869));
#8802=CARTESIAN_POINT('Ctrl Pts',(-0.115082411738962,-0.158311560806047,
2.12291016041925));
#8803=CARTESIAN_POINT('Ctrl Pts',(-0.0627617170802516,-0.196345370183675,
2.12661506471318));
#8804=CARTESIAN_POINT('Ctrl Pts',(0.0102790582366786,-0.205875881267149,
2.1303199690071));
#8805=CARTESIAN_POINT('Ctrl Pts',(0.0706073005241847,-0.182540737619698,
2.13402487330103));
#8806=CARTESIAN_POINT('Ctrl Pts',(0.130935542811693,-0.159205593972247,
2.13772977759495));
#8807=CARTESIAN_POINT('Ctrl Pts',(0.178551252069776,-0.103004795593869,
2.14143468188888));
#8808=CARTESIAN_POINT('Ctrl Pts',(0.191659511540249,-0.0396628720499632,
2.1451395861828));
#8809=CARTESIAN_POINT('Ctrl Pts',(0.204767771010722,0.0236790514939429,
2.14884449047673));
#8810=CARTESIAN_POINT('Ctrl Pts',(0.183368580693586,0.0941621002033779,
2.15254939477065));
#8811=CARTESIAN_POINT('Ctrl Pts',(0.137256892346912,0.139524396685099,2.15625429906458));
#8812=CARTESIAN_POINT('Ctrl Pts',(0.091145204000239,0.184886693166819,2.1599592033585));
#8813=CARTESIAN_POINT('Ctrl Pts',(0.02032101762403,0.205128237420826,2.16366410765243));
#8814=CARTESIAN_POINT('Ctrl Pts',(-0.0427976421750205,0.190983961646384,
2.16736901194635));
#8815=CARTESIAN_POINT('Ctrl Pts',(-0.105916301974075,0.176839685871941,
2.17107391624028));
#8816=CARTESIAN_POINT('Ctrl Pts',(-0.161329435195969,0.128309590069043,
2.1747788205342));
#8817=CARTESIAN_POINT('Ctrl Pts',(-0.183673046253887,0.0676071289816255,
2.17848372482813));
#8818=CARTESIAN_POINT('Ctrl Pts',(-0.191572025293587,0.0461474165589195,
2.17979349348128));
#8819=CARTESIAN_POINT('Ctrl Pts',(-0.195338026112343,0.023166420569767,
2.18110326213443));
#8820=CARTESIAN_POINT('Ctrl Pts',(-0.19518796491764,0.000137929913403057,
2.18241303078758));
#8821=CARTESIAN_POINT('Origin',(0.,0.,0.));
#8822=CARTESIAN_POINT('',(-0.195174657492043,-0.000131013293013224,2.26258696921242));
#8823=CARTESIAN_POINT('',(-0.195195111391083,-0.000141315875587933,2.25241303078758));
#8824=CARTESIAN_POINT('',(-0.1954,-2.39295984553393E-17,0.));
#8825=CARTESIAN_POINT('Ctrl Pts',(-0.195174657492043,-0.000131013293013224,
2.26258696921242));
#8826=CARTESIAN_POINT('Ctrl Pts',(-0.194918943248225,0.0413594787080526,
2.26022755698725));
#8827=CARTESIAN_POINT('Ctrl Pts',(-0.181975540580321,0.0829956888567188,
2.25786814476208));
#8828=CARTESIAN_POINT('Ctrl Pts',(-0.157529455112694,0.116150705603978,
2.25550873253691));
#8829=CARTESIAN_POINT('Ctrl Pts',(-0.119142603483941,0.168212894059927,
2.25180382824299));
#8830=CARTESIAN_POINT('Ctrl Pts',(-0.052393188412561,0.199362710149808,
2.24809892394906));
#8831=CARTESIAN_POINT('Ctrl Pts',(0.0121657881897227,0.195342029196137,
2.24439401965513));
#8832=CARTESIAN_POINT('Ctrl Pts',(0.0767247647920027,0.191321348242465,
2.24068911536121));
#8833=CARTESIAN_POINT('Ctrl Pts',(0.139093302925189,0.152130170245245,2.23698421106728));
#8834=CARTESIAN_POINT('Ctrl Pts',(0.170723796521274,0.095707324392732,2.23327930677336));
#8835=CARTESIAN_POINT('Ctrl Pts',(0.202354290117362,0.0392844785402158,
2.22957440247943));
#8836=CARTESIAN_POINT('Ctrl Pts',(0.203246739176347,-0.0343700351675917,
2.22586949818551));
#8837=CARTESIAN_POINT('Ctrl Pts',(0.17299261862985,-0.0915426972318238,
2.22216459389158));
#8838=CARTESIAN_POINT('Ctrl Pts',(0.142738498083355,-0.148715359296053,
2.21845968959766));
#8839=CARTESIAN_POINT('Ctrl Pts',(0.0813378079313799,-0.189406169716704,
2.21475478530373));
#8840=CARTESIAN_POINT('Ctrl Pts',(0.0168952149404143,-0.194989904088049,
2.21104988100981));
#8841=CARTESIAN_POINT('Ctrl Pts',(-0.0475473780505532,-0.200573638459395,
2.20734497671588));
#8842=CARTESIAN_POINT('Ctrl Pts',(-0.115031873880513,-0.171050296781432,
2.20364007242196));
#8843=CARTESIAN_POINT('Ctrl Pts',(-0.154668916633727,-0.119933465587592,
2.19993516812803));
#8844=CARTESIAN_POINT('Ctrl Pts',(-0.180873900754785,-0.0861389224857415,
2.19748576848949));
#8845=CARTESIAN_POINT('Ctrl Pts',(-0.194907197410721,-0.0429062018620786,
2.19503636885096));
#8846=CARTESIAN_POINT('Ctrl Pts',(-0.195209426648116,0.000147489598137318,
2.19258696921242));
#8847=CARTESIAN_POINT('Ctrl Pts',(-0.19518796491764,0.000137929913403057,
2.18241303078758));
#8848=CARTESIAN_POINT('Ctrl Pts',(-0.194913552398402,-0.0419735976389966,
2.18480816642835));
#8849=CARTESIAN_POINT('Ctrl Pts',(-0.181543684570605,-0.0842439491042262,
2.18720330206913));
#8850=CARTESIAN_POINT('Ctrl Pts',(-0.156404834897329,-0.117660695730726,
2.18959843770991));
#8851=CARTESIAN_POINT('Ctrl Pts',(-0.117518923588915,-0.169351232983719,
2.19330334200383));
#8852=CARTESIAN_POINT('Ctrl Pts',(-0.0504730120781484,-0.199857481117771,
2.19700824629776));
#8853=CARTESIAN_POINT('Ctrl Pts',(0.0140442882391665,-0.195215956814723,
2.20071315059168));
#8854=CARTESIAN_POINT('Ctrl Pts',(0.0785615885564833,-0.190574432511675,
2.20441805488561));
#8855=CARTESIAN_POINT('Ctrl Pts',(0.140550277680348,-0.150785135771524,
2.20812295917953));
#8856=CARTESIAN_POINT('Ctrl Pts',(0.171636559439807,-0.0940606369606153,
2.21182786347346));
#8857=CARTESIAN_POINT('Ctrl Pts',(0.202722841199266,-0.0373361381497062,
2.21553276776738));
#8858=CARTESIAN_POINT('Ctrl Pts',(0.202906715594321,0.0363235627319613,
2.21923767206131));
#8859=CARTESIAN_POINT('Ctrl Pts',(0.17210402315838,0.0932025559367594,2.22294257635524));
#8860=CARTESIAN_POINT('Ctrl Pts',(0.14130133072244,0.150081549141557,2.22664748064916));
#8861=CARTESIAN_POINT('Ctrl Pts',(0.0795120714555056,0.190179834669486,
2.23035238494309));
#8862=CARTESIAN_POINT('Ctrl Pts',(0.0150187464949281,0.195143407566839,
2.23405728923701));
#8863=CARTESIAN_POINT('Ctrl Pts',(-0.0494745784656475,0.200106980464191,
2.23776219353094));
#8864=CARTESIAN_POINT('Ctrl Pts',(-0.116671969119866,0.16993584073097,2.24146709782486));
#8865=CARTESIAN_POINT('Ctrl Pts',(-0.155815460686541,0.118440090365932,
2.24517200211879));
#8866=CARTESIAN_POINT('Ctrl Pts',(-0.181316717232319,0.0848915670095187,
2.24758567834172));
#8867=CARTESIAN_POINT('Ctrl Pts',(-0.194911113219737,0.0422922816017406,
2.24999935456465));
#8868=CARTESIAN_POINT('Ctrl Pts',(-0.195195111391083,-0.000141315875587933,
2.25241303078758));
#8869=CARTESIAN_POINT('Origin',(0.,0.,0.));
#8870=CARTESIAN_POINT('',(-0.195681353759257,-7.39606064390219E-5,2.33258696921242));
#8871=CARTESIAN_POINT('',(-0.195697752751996,-5.95341972371984E-5,2.32241303078758));
#8872=CARTESIAN_POINT('',(-0.1954,-2.39295984553393E-17,0.));
#8873=CARTESIAN_POINT('Ctrl Pts',(-0.195681353759257,-7.39606064390219E-5,
2.33258696921242));
#8874=CARTESIAN_POINT('Ctrl Pts',(-0.195380276086469,0.060422861610312,
2.32912364941747));
#8875=CARTESIAN_POINT('Ctrl Pts',(-0.165164977787156,0.12117446104776,2.32566032962252));
#8876=CARTESIAN_POINT('Ctrl Pts',(-0.11660138687175,0.157196309339772,2.32219700982757));
#8877=CARTESIAN_POINT('Ctrl Pts',(-0.0646502338846034,0.195730868177439,
2.31849210553364));
#8878=CARTESIAN_POINT('Ctrl Pts',(0.00829826751356548,0.205965289678994,
2.31478720123972));
#8879=CARTESIAN_POINT('Ctrl Pts',(0.0688488487742365,0.183211962286636,
2.31108229694579));
#8880=CARTESIAN_POINT('Ctrl Pts',(0.129399430034907,0.160458634894278,2.30737739265187));
#8881=CARTESIAN_POINT('Ctrl Pts',(0.177552091158081,0.104717558608008,2.30367248835794));
#8882=CARTESIAN_POINT('Ctrl Pts',(0.191268709972338,0.0415044437598955,
2.29996758406402));
#8883=CARTESIAN_POINT('Ctrl Pts',(0.204985328786596,-0.0217086710882173,
2.29626267977009));
#8884=CARTESIAN_POINT('Ctrl Pts',(0.184265905291938,-0.0923938244981725,
2.29255777547616));
#8885=CARTESIAN_POINT('Ctrl Pts',(0.138592893132747,-0.138197475482013,
2.28885287118224));
#8886=CARTESIAN_POINT('Ctrl Pts',(0.0929198809735568,-0.184001126465853,
2.28514796688831));
#8887=CARTESIAN_POINT('Ctrl Pts',(0.0222932801498333,-0.204923275023578,
2.28144306259439));
#8888=CARTESIAN_POINT('Ctrl Pts',(-0.0409586140019971,-0.19138687945489,
2.27773815830046));
#8889=CARTESIAN_POINT('Ctrl Pts',(-0.104210508153827,-0.177850483886201,
2.27403325400654));
#8890=CARTESIAN_POINT('Ctrl Pts',(-0.160087695633765,-0.1298555441911,2.27032834971261));
#8891=CARTESIAN_POINT('Ctrl Pts',(-0.18301414528067,-0.0693707939325425,
2.26662344541869));
#8892=CARTESIAN_POINT('Ctrl Pts',(-0.191340232466025,-0.0474048414281955,
2.26527795334993));
#8893=CARTESIAN_POINT('Ctrl Pts',(-0.195320482576467,-0.0237916213548985,
2.26393246128118));
#8894=CARTESIAN_POINT('Ctrl Pts',(-0.195174657492043,-0.000131013293013224,
2.26258696921242));
#8895=CARTESIAN_POINT('Ctrl Pts',(-0.195195111391083,-0.000141315875587933,
2.25241303078758));
#8896=CARTESIAN_POINT('Ctrl Pts',(-0.195347039975153,-0.0228417309915556,
2.25370425885857));
#8897=CARTESIAN_POINT('Ctrl Pts',(-0.191689723357918,-0.045494728595087,
2.25499548692957));
#8898=CARTESIAN_POINT('Ctrl Pts',(-0.184008281643019,-0.0666892810800291,
2.25628671500056));
#8899=CARTESIAN_POINT('Ctrl Pts',(-0.16196801855369,-0.127502541164088,
2.25999161929449));
#8900=CARTESIAN_POINT('Ctrl Pts',(-0.106797899895904,-0.17630870033535,
2.26369652358841));
#8901=CARTESIAN_POINT('Ctrl Pts',(-0.0437506280009387,-0.190767918158648,
2.26740142788234));
#8902=CARTESIAN_POINT('Ctrl Pts',(0.0192966438940271,-0.205227135981945,
2.27110633217626));
#8903=CARTESIAN_POINT('Ctrl Pts',(0.0902210690261749,-0.185339412457277,
2.27481123647019));
#8904=CARTESIAN_POINT('Ctrl Pts',(0.136558628570232,-0.140207909463584,
2.27851614076412));
#8905=CARTESIAN_POINT('Ctrl Pts',(0.182896188114289,-0.0950764064698918,
2.28222104505804));
#8906=CARTESIAN_POINT('Ctrl Pts',(0.204646882070257,-0.0247011240071736,
2.28592594935197));
#8907=CARTESIAN_POINT('Ctrl Pts',(0.191855080140027,0.0387054769946518,
2.28963085364589));
#8908=CARTESIAN_POINT('Ctrl Pts',(0.179063278209797,0.102112077996479,2.29333575793982));
#8909=CARTESIAN_POINT('Ctrl Pts',(0.131728980393372,0.15854999753741,2.29704066223374));
#8910=CARTESIAN_POINT('Ctrl Pts',(0.0715178881091697,0.182186000086743,
2.30074556652767));
#8911=CARTESIAN_POINT('Ctrl Pts',(0.0113067958249691,0.205822002636076,
2.30445047082159));
#8912=CARTESIAN_POINT('Ctrl Pts',(-0.0617810909270064,0.196656088193809,
2.30815537511552));
#8913=CARTESIAN_POINT('Ctrl Pts',(-0.114290821684253,0.15888405075463,2.31186027940945));
#8914=CARTESIAN_POINT('Ctrl Pts',(-0.164145652799363,0.123021773034915,
2.31537786320216));
#8915=CARTESIAN_POINT('Ctrl Pts',(-0.195450592530455,0.0613729051733717,
2.31889544699487));
#8916=CARTESIAN_POINT('Ctrl Pts',(-0.195697752751996,-5.95341972371984E-5,
2.32241303078758));
#8917=CARTESIAN_POINT('Origin',(0.,0.,0.));
#8918=CARTESIAN_POINT('',(-0.1954,-2.39295984553393E-17,2.4));
#8919=CARTESIAN_POINT('',(-0.195373070919361,0.000178101583232409,2.39241303078758));
#8920=CARTESIAN_POINT('',(-0.1954,-2.39295984553393E-17,0.));
#8921=CARTESIAN_POINT('',(-0.190155688860645,0.0449663651403318,2.4));
#8922=CARTESIAN_POINT('Origin',(0.,0.,2.4));
#8923=CARTESIAN_POINT('Ctrl Pts',(-0.190155688860645,0.0449663651403318,
2.4));
#8924=CARTESIAN_POINT('Ctrl Pts',(-0.175202059751608,0.108202911730688,
2.39629509570607));
#8925=CARTESIAN_POINT('Ctrl Pts',(-0.126357437987047,0.162847509466655,
2.39259019141215));
#8926=CARTESIAN_POINT('Ctrl Pts',(-0.0654921592886404,0.184422161949795,
2.38888528711823));
#8927=CARTESIAN_POINT('Ctrl Pts',(-0.00462688059022985,0.205996814432936,
2.3851803828243));
#8928=CARTESIAN_POINT('Ctrl Pts',(0.0682590550420274,0.194501521663244,
2.38147547853037));
#8929=CARTESIAN_POINT('Ctrl Pts',(0.119524669012765,0.15503197640457,2.37777057423645));
#8930=CARTESIAN_POINT('Ctrl Pts',(0.1707902829835,0.115562431145897,2.37406566994252));
#8931=CARTESIAN_POINT('Ctrl Pts',(0.200435575292716,0.0481186333982456,
2.3703607656486));
#8932=CARTESIAN_POINT('Ctrl Pts',(0.195018846313631,-0.0163501344389201,
2.36665586135467));
#8933=CARTESIAN_POINT('Ctrl Pts',(0.189602117334546,-0.0808189022760859,
2.36295095706075));
#8934=CARTESIAN_POINT('Ctrl Pts',(0.149123367067157,-0.142312640202767,
2.35924605276682));
#8935=CARTESIAN_POINT('Ctrl Pts',(0.0920460129031269,-0.172724421142238,
2.3555411484729));
#8936=CARTESIAN_POINT('Ctrl Pts',(0.0349686587390981,-0.203136202081708,
2.35183624417897));
#8937=CARTESIAN_POINT('Ctrl Pts',(-0.0387072993215716,-0.202466026033974,
2.34813133988505));
#8938=CARTESIAN_POINT('Ctrl Pts',(-0.0952247602900568,-0.170999569986643,
2.34442643559112));
#8939=CARTESIAN_POINT('Ctrl Pts',(-0.151742221258544,-0.139533113939311,
2.34072153129719));
#8940=CARTESIAN_POINT('Ctrl Pts',(-0.191101185134843,-0.0772703778923819,
2.33701662700327));
#8941=CARTESIAN_POINT('Ctrl Pts',(-0.195303764784931,-0.0127216617820273,
2.33331172270934));
#8942=CARTESIAN_POINT('Ctrl Pts',(-0.195577801040289,-0.00851265447608656,
2.33307013821037));
#8943=CARTESIAN_POINT('Ctrl Pts',(-0.195702355486801,-0.0042939273868865,
2.3328285537114));
#8944=CARTESIAN_POINT('Ctrl Pts',(-0.195681353759257,-7.39606064390219E-5,
2.33258696921242));
#8945=CARTESIAN_POINT('Ctrl Pts',(-0.195697752751996,-5.95341972371984E-5,
2.32241303078758));
#8946=CARTESIAN_POINT('Ctrl Pts',(-0.195710914677712,-0.00333097164176583,
2.32260035128879));
#8947=CARTESIAN_POINT('Ctrl Pts',(-0.195636001710979,-0.00660179532972963,
2.32278767179001));
#8948=CARTESIAN_POINT('Ctrl Pts',(-0.195471124962234,-0.0098680783927403,
2.32297499229122));
#8949=CARTESIAN_POINT('Ctrl Pts',(-0.192210122720448,-0.0744700096648406,
2.32667989658515));
#8950=CARTESIAN_POINT('Ctrl Pts',(-0.153756543474356,-0.137295711772949,
2.33038480087907));
#8951=CARTESIAN_POINT('Ctrl Pts',(-0.0977087684767672,-0.169587100981169,
2.334089705173));
#8952=CARTESIAN_POINT('Ctrl Pts',(-0.0416609934791779,-0.20187849018939,
2.33779460946692));
#8953=CARTESIAN_POINT('Ctrl Pts',(0.0319809772699075,-0.203635566497722,
2.34149951376085));
#8954=CARTESIAN_POINT('Ctrl Pts',(0.0895040276926783,-0.174056293370152,
2.34520441805477));
#8955=CARTESIAN_POINT('Ctrl Pts',(0.147027078115449,-0.144477020242583,
2.3489093223487));
#8956=CARTESIAN_POINT('Ctrl Pts',(0.188431208211903,-0.0835613976791124,
2.35261422664262));
#8957=CARTESIAN_POINT('Ctrl Pts',(0.194774820151305,-0.0191878227159973,
2.35631913093655));
#8958=CARTESIAN_POINT('Ctrl Pts',(0.201118432090707,0.045185752247116,2.36002403523048));
#8959=CARTESIAN_POINT('Ctrl Pts',(0.172401525873055,0.113017279609876,2.3637289395244));
#8960=CARTESIAN_POINT('Ctrl Pts',(0.121749293910871,0.153250507222424,2.36743384381833));
#8961=CARTESIAN_POINT('Ctrl Pts',(0.0710970619486833,0.193483734834974,
2.37113874811225));
#8962=CARTESIAN_POINT('Ctrl Pts',(-0.00149049575803851,0.206118662697314,
2.37484365240618));
#8963=CARTESIAN_POINT('Ctrl Pts',(-0.0627515027614027,0.185387280299844,
2.3785485567001));
#8964=CARTESIAN_POINT('Ctrl Pts',(-0.124012509764765,0.164655897902375,
2.38225346099403));
#8965=CARTESIAN_POINT('Ctrl Pts',(-0.173946966064769,0.1105582052451,2.38595836528795));
#8966=CARTESIAN_POINT('Ctrl Pts',(-0.189769007749096,0.0478268239240077,
2.38966326958188));
#8967=CARTESIAN_POINT('Ctrl Pts',(-0.193683354154737,0.0323071860735817,
2.39057985665045));
#8968=CARTESIAN_POINT('Ctrl Pts',(-0.19550981867675,0.0162591153240736,
2.39149644371901));
#8969=CARTESIAN_POINT('Ctrl Pts',(-0.195373070919361,0.000178101583232409,
2.39241303078758));
#8970=CARTESIAN_POINT('Origin',(0.,0.,-0.129405622560373));
#8971=CARTESIAN_POINT('',(-0.155773974295048,-5.88770334001961E-5,2.35559437743962));
#8972=CARTESIAN_POINT('',(-0.155528562853156,0.000141779433378626,2.36940562256037));
#8973=CARTESIAN_POINT('',(-0.15555,4.36677073508985E-14,-0.129405622560373));
#8974=CARTESIAN_POINT('',(0.103461089470168,0.116496783315852,2.4));
#8975=CARTESIAN_POINT('Ctrl Pts',(-0.155773974295048,-5.88770334001795E-5,
2.35559437743962));
#8976=CARTESIAN_POINT('Ctrl Pts',(-0.15579069291695,-0.00341822111067628,
2.3558359619386));
#8977=CARTESIAN_POINT('Ctrl Pts',(-0.154170948464013,-0.0582798498405871,
2.3597824507315));
#8978=CARTESIAN_POINT('Ctrl Pts',(-0.0894637445537859,-0.160641476281263,
2.36743384381833));
#8979=CARTESIAN_POINT('Ctrl Pts',(0.0864875647042136,-0.162241976039076,
2.3785485567001));
#8980=CARTESIAN_POINT('Ctrl Pts',(0.180902522808575,-0.0188104557555769,
2.38940394209399));
#8981=CARTESIAN_POINT('Ctrl Pts',(0.139126171174338,0.0844901197987813,
2.39655442319396));
#8982=CARTESIAN_POINT('Ctrl Pts',(0.103461767481305,0.116497970106856,2.4));
#8983=CARTESIAN_POINT('',(0.143545299885862,-0.0599211930845659,2.4));
#8984=CARTESIAN_POINT('Origin',(0.,0.,2.4));
#8985=CARTESIAN_POINT('Ctrl Pts',(-0.155528562853156,0.00014177943337863,
2.36940562256037));
#8986=CARTESIAN_POINT('Ctrl Pts',(-0.155197405712005,-0.0388010349799734,
2.37219393978573));
#8987=CARTESIAN_POINT('Ctrl Pts',(-0.120746574532385,-0.130053255016983,
2.37868716130501));
#8988=CARTESIAN_POINT('Ctrl Pts',(0.0327466243405011,-0.180863000230457,
2.38888528711822));
#8989=CARTESIAN_POINT('Ctrl Pts',(0.123618421332056,-0.107657388085867,
2.39629509570608));
#8990=CARTESIAN_POINT('Ctrl Pts',(0.143545299885864,-0.0599211930845618,
2.4));
#8991=CARTESIAN_POINT('Origin',(0.,0.,-0.129405622560373));
#8992=CARTESIAN_POINT('',(-0.155370613986117,-0.00010429435887339,2.28559437743963));
#8993=CARTESIAN_POINT('',(-0.155787028866801,-4.73927552151754E-5,2.29940562256037));
#8994=CARTESIAN_POINT('',(-0.15555,4.36677073508985E-14,-0.129405622560373));
#8995=CARTESIAN_POINT('Ctrl Pts',(-0.155370613986117,-0.000104294358873382,
2.28559437743963));
#8996=CARTESIAN_POINT('Ctrl Pts',(-0.155486699410286,-0.0189395429977021,
2.28693986950838));
#8997=CARTESIAN_POINT('Ctrl Pts',(-0.143593460567012,-0.0894973367036735,
2.29199026587106));
#8998=CARTESIAN_POINT('Ctrl Pts',(-0.0384761925835495,-0.179786364575594,
2.30074556652767));
#8999=CARTESIAN_POINT('Ctrl Pts',(0.130192708513641,-0.129820547664333,
2.31186027940944));
#9000=CARTESIAN_POINT('Ctrl Pts',(0.179674381869752,0.0389881874367674,
2.32297499229122));
#9001=CARTESIAN_POINT('Ctrl Pts',(0.0646772513010348,0.172107804882976,
2.33408970517299));
#9002=CARTESIAN_POINT('Ctrl Pts',(-0.105750122905907,0.14819743592946,2.3449628335558));
#9003=CARTESIAN_POINT('Ctrl Pts',(-0.155534298593903,0.0481001848694375,
2.35213105764467));
#9004=CARTESIAN_POINT('Ctrl Pts',(-0.155773974295048,-5.88770334001795E-5,
2.35559437743962));
#9005=CARTESIAN_POINT('Ctrl Pts',(-0.155787028866801,-4.73927552151962E-5,
2.29940562256037));
#9006=CARTESIAN_POINT('Ctrl Pts',(-0.155797506541035,-0.00265165117128265,
2.29959294306158));
#9007=CARTESIAN_POINT('Ctrl Pts',(-0.154558381720229,-0.0567538846432019,
2.30348516785672));
#9008=CARTESIAN_POINT('Ctrl Pts',(-0.0917880045327959,-0.15930852573796,
2.31108229694579));
#9009=CARTESIAN_POINT('Ctrl Pts',(0.0840821369721223,-0.163504736890904,
2.32219700982757));
#9010=CARTESIAN_POINT('Ctrl Pts',(0.182962573561233,-0.0180273813676558,
2.33331172270934));
#9011=CARTESIAN_POINT('Ctrl Pts',(0.114381487141248,0.143966386512752,2.34442643559112));
#9012=CARTESIAN_POINT('Ctrl Pts',(-0.0589705282315283,0.174140844480832,
2.35554114847289));
#9013=CARTESIAN_POINT('Ctrl Pts',(-0.148306390161892,0.0773566926129291,
2.36386754412931));
#9014=CARTESIAN_POINT('Ctrl Pts',(-0.155637422186119,0.0129432210269571,
2.3684890354918));
#9015=CARTESIAN_POINT('Ctrl Pts',(-0.155528562853156,0.00014177943337863,
2.36940562256037));
#9016=CARTESIAN_POINT('Origin',(0.,0.,-0.129405622560373));
#9017=CARTESIAN_POINT('',(-0.155398292298436,0.000117410475919154,2.21559437743963));
#9018=CARTESIAN_POINT('',(-0.155386896504006,-0.000112495826188885,2.22940562256037));
#9019=CARTESIAN_POINT('',(-0.15555,4.36677073508985E-14,-0.129405622560373));
#9020=CARTESIAN_POINT('Ctrl Pts',(-0.155398292298436,0.000117410475919153,
2.21559437743963));
#9021=CARTESIAN_POINT('Ctrl Pts',(-0.155157699883514,-0.0341558838262174,
2.21804377707816));
#9022=CARTESIAN_POINT('Ctrl Pts',(-0.12708886065999,-0.120628244108591,
2.22419808101062));
#9023=CARTESIAN_POINT('Ctrl Pts',(0.0158711293274525,-0.18317085598959,
2.23405728923701));
#9024=CARTESIAN_POINT('Ctrl Pts',(0.162506912640762,-0.0859939538258468,
2.24517200211879));
#9025=CARTESIAN_POINT('Ctrl Pts',(0.160375585346118,0.0899061424983564,
2.25628671500056));
#9026=CARTESIAN_POINT('Ctrl Pts',(0.011428408683624,0.183501655356106,2.26740142788234));
#9027=CARTESIAN_POINT('Ctrl Pts',(-0.128683759207511,0.11811579007031,2.27717064869536));
#9028=CARTESIAN_POINT('Ctrl Pts',(-0.155167050267454,0.032924600373803,
2.28323496521446));
#9029=CARTESIAN_POINT('Ctrl Pts',(-0.155370613986117,-0.000104294358873382,
2.28559437743963));
#9030=CARTESIAN_POINT('Ctrl Pts',(-0.155386896504006,-0.000112495826188891,
2.22940562256037));
#9031=CARTESIAN_POINT('Ctrl Pts',(-0.155507840676234,-0.0181833738778352,
2.23069685063136));
#9032=CARTESIAN_POINT('Ctrl Pts',(-0.144242638453781,-0.0879587380741699,
2.23569298299629));
#9033=CARTESIAN_POINT('Ctrl Pts',(-0.0410987787696598,-0.179204792201909,
2.24439401965513));
#9034=CARTESIAN_POINT('Ctrl Pts',(0.128281379817428,-0.13170936649677,2.25550873253691));
#9035=CARTESIAN_POINT('Ctrl Pts',(0.18022591070051,0.0363593415954858,2.26662344541869));
#9036=CARTESIAN_POINT('Ctrl Pts',(0.0671831774557089,0.171143144838974,
2.27773815830046));
#9037=CARTESIAN_POINT('Ctrl Pts',(-0.104422007378309,0.149622226504381,
2.28866555068102));
#9038=CARTESIAN_POINT('Ctrl Pts',(-0.155590274657669,0.0488564759453739,
2.29588803876766));
#9039=CARTESIAN_POINT('Ctrl Pts',(-0.155787028866801,-4.73927552151962E-5,
2.29940562256037));
#9040=CARTESIAN_POINT('Origin',(0.,0.,-0.129405622560373));
#9041=CARTESIAN_POINT('',(-0.155793317189999,3.87877782857977E-5,2.14559437743963));
#9042=CARTESIAN_POINT('',(-0.155381207486893,0.000109800399387149,2.15940562256037));
#9043=CARTESIAN_POINT('',(-0.15555,4.36677073508985E-14,-0.129405622560373));
#9044=CARTESIAN_POINT('Ctrl Pts',(-0.155793317189999,3.87877782858049E-5,
2.14559437743963));
#9045=CARTESIAN_POINT('Ctrl Pts',(-0.155627927476026,-0.0493566447310424,
2.14914768464794));
#9046=CARTESIAN_POINT('Ctrl Pts',(-0.103538872562762,-0.150555101055555,
2.15640589615019));
#9047=CARTESIAN_POINT('Ctrl Pts',(0.0688260039060977,-0.170488812072594,
2.16736901194635));
#9048=CARTESIAN_POINT('Ctrl Pts',(0.180567516503863,-0.0346240655854127,
2.17848372482813));
#9049=CARTESIAN_POINT('Ctrl Pts',(0.127008372351303,0.132937304665343,2.18959843770991));
#9050=CARTESIAN_POINT('Ctrl Pts',(-0.0428206707452402,0.178801130147604,
2.20071315059168));
#9051=CARTESIAN_POINT('Ctrl Pts',(-0.144662237131258,0.0869458188293342,
2.20937846383492));
#9052=CARTESIAN_POINT('Ctrl Pts',(-0.155521614312629,0.017685095175004,
2.21433887278424));
#9053=CARTESIAN_POINT('Ctrl Pts',(-0.155398292298436,0.000117410475919153,
2.21559437743963));
#9054=CARTESIAN_POINT('Ctrl Pts',(-0.155381207486893,0.000109800399387143,
2.15940562256037));
#9055=CARTESIAN_POINT('Ctrl Pts',(-0.15516275883098,-0.0334134755001949,
2.16180075820114));
#9056=CARTESIAN_POINT('Ctrl Pts',(-0.128056153355666,-0.119114078918986,
2.16790079813585));
#9057=CARTESIAN_POINT('Ctrl Pts',(0.013193011805229,-0.183383204120377,
2.17770574236448));
#9058=CARTESIAN_POINT('Ctrl Pts',(0.161233041383799,-0.0883592771818423,
2.18882045524625));
#9059=CARTESIAN_POINT('Ctrl Pts',(0.161672166186531,0.08755320703735,2.19993516812803));
#9060=CARTESIAN_POINT('Ctrl Pts',(0.0141084106240242,0.183315054230848,
2.2110498810098));
#9061=CARTESIAN_POINT('Ctrl Pts',(-0.127727581106385,0.119631725398659,
2.22087336582059));
#9062=CARTESIAN_POINT('Ctrl Pts',(-0.155160817099938,0.0336671668534186,
2.22699194633744));
#9063=CARTESIAN_POINT('Ctrl Pts',(-0.155386896504006,-0.000112495826188891,
2.22940562256037));
#9064=CARTESIAN_POINT('Origin',(0.,0.,-0.129405622560373));
#9065=CARTESIAN_POINT('',(-0.155512395363828,-0.000141626737826867,2.07559437743963));
#9066=CARTESIAN_POINT('',(-0.155783925033264,5.20139628275244E-5,2.08940562256037));
#9067=CARTESIAN_POINT('',(-0.15555,4.36677073508985E-14,-0.129405622560373));
#9068=CARTESIAN_POINT('Ctrl Pts',(-0.155512395363828,-0.000141626737826864,
2.07559437743963));
#9069=CARTESIAN_POINT('Ctrl Pts',(-0.155631529586225,-0.0134421217799902,
2.0765466879238));
#9070=CARTESIAN_POINT('Ctrl Pts',(-0.147981681918013,-0.0783523864199532,
2.0812039027019));
#9071=CARTESIAN_POINT('Ctrl Pts',(-0.0572598509893232,-0.174713374727145,
2.08956602177392));
#9072=CARTESIAN_POINT('Ctrl Pts',(0.115743835073967,-0.142852436054201,
2.10068073465569));
#9073=CARTESIAN_POINT('Ctrl Pts',(0.182789748630034,0.0197828623436046,
2.11179544753748));
#9074=CARTESIAN_POINT('Ctrl Pts',(0.0825006624943804,0.164307925944582,
2.12291016041925));
#9075=CARTESIAN_POINT('Ctrl Pts',(-0.0933137111781269,0.15841718704366,
2.13402487330103));
#9076=CARTESIAN_POINT('Ctrl Pts',(-0.154806754983662,0.0557495847898722,
2.14158627897448));
#9077=CARTESIAN_POINT('Ctrl Pts',(-0.155800373320291,0.00214617764686899,
2.14544278035402));
#9078=CARTESIAN_POINT('Ctrl Pts',(-0.155793317189999,3.87877782858049E-5,
2.14559437743963));
#9079=CARTESIAN_POINT('Ctrl Pts',(-0.155783925033264,5.201396282752E-5,
2.08940562256037));
#9080=CARTESIAN_POINT('Ctrl Pts',(-0.155572294092276,-0.0485969103211591,
2.09290466577093));
#9081=CARTESIAN_POINT('Ctrl Pts',(-0.104876060672191,-0.149137277709018,
2.10010861327541));
#9082=CARTESIAN_POINT('Ctrl Pts',(0.0663275338242693,-0.17147627599867,
2.11101746507382));
#9083=CARTESIAN_POINT('Ctrl Pts',(0.180042327710072,-0.0372587603217594,
2.1221321779556));
#9084=CARTESIAN_POINT('Ctrl Pts',(0.128937250118005,0.131067312760423,2.13324689083737));
#9085=CARTESIAN_POINT('Ctrl Pts',(-0.0402035204677608,0.179407725381376,
2.14436160371915));
#9086=CARTESIAN_POINT('Ctrl Pts',(-0.144022462459615,0.0884844566890199,
2.15308118096014));
#9087=CARTESIAN_POINT('Ctrl Pts',(-0.155500665106314,0.0184418460574962,
2.15809585390722));
#9088=CARTESIAN_POINT('Ctrl Pts',(-0.155381207486893,0.000109800399387143,
2.15940562256037));
#9089=CARTESIAN_POINT('Origin',(0.,0.,-0.129405622560373));
#9090=CARTESIAN_POINT('',(-0.155307392249976,4.6077661301668E-5,2.00559437743963));
#9091=CARTESIAN_POINT('',(-0.155535029491756,-0.000142310086639022,2.01940562256037));
#9092=CARTESIAN_POINT('',(-0.15555,4.36677073508985E-14,-0.129405622560373));
#9093=CARTESIAN_POINT('Ctrl Pts',(-0.155307392249976,4.60776613016665E-5,
2.00559437743963));
#9094=CARTESIAN_POINT('Ctrl Pts',(-0.155230909498638,-0.0287678470951232,
2.00765059549358));
#9095=CARTESIAN_POINT('Ctrl Pts',(-0.133719279780215,-0.109604980011744,
2.01341171784146));
#9096=CARTESIAN_POINT('Ctrl Pts',(-0.00357486400063734,-0.183822398504055,
2.02287774448326));
#9097=CARTESIAN_POINT('Ctrl Pts',(0.152509256593582,-0.102685833967865,
2.03399245736504));
#9098=CARTESIAN_POINT('Ctrl Pts',(0.168978674541131,0.072454547095341,2.04510717024682));
#9099=CARTESIAN_POINT('Ctrl Pts',(0.0307564499829109,0.181266363754544,
2.05622188312859));
#9100=CARTESIAN_POINT('Ctrl Pts',(-0.121366472017063,0.129032552536754,
2.0663842855262));
#9101=CARTESIAN_POINT('Ctrl Pts',(-0.155168045355556,0.0383026211499949,
2.07284178362987));
#9102=CARTESIAN_POINT('Ctrl Pts',(-0.155512395363828,-0.000141626737826864,
2.07559437743963));
#9103=CARTESIAN_POINT('Ctrl Pts',(-0.155535029491756,-0.000142310086639015,
2.01940562256037));
#9104=CARTESIAN_POINT('Ctrl Pts',(-0.155649341554365,-0.0126802716132022,
2.02030366904678));
#9105=CARTESIAN_POINT('Ctrl Pts',(-0.148531226312109,-0.0768156130876391,
2.02490661982712));
#9106=CARTESIAN_POINT('Ctrl Pts',(-0.0598065907447483,-0.173858064744653,
2.03321447490139));
#9107=CARTESIAN_POINT('Ctrl Pts',(0.113644170098336,-0.144528397126456,
2.04432918778316));
#9108=CARTESIAN_POINT('Ctrl Pts',(0.183059298154547,0.0171098899136208,
2.05544390066494));
#9109=CARTESIAN_POINT('Ctrl Pts',(0.0848926672411447,0.163084916597067,
2.06655861354672));
#9110=CARTESIAN_POINT('Ctrl Pts',(-0.0909890136144577,0.159763745495145,
2.07767332642849));
#9111=CARTESIAN_POINT('Ctrl Pts',(-0.154427657211485,0.0572753556709789,
2.08528899609971));
#9112=CARTESIAN_POINT('Ctrl Pts',(-0.155796376029769,0.00291420218260239,
2.089199761477));
#9113=CARTESIAN_POINT('Ctrl Pts',(-0.155783925033264,5.201396282752E-5,
2.08940562256037));
#9114=CARTESIAN_POINT('Origin',(0.,0.,-0.129405622560373));
#9115=CARTESIAN_POINT('',(-0.155681301642334,0.000117756784957254,1.93559437743963));
#9116=CARTESIAN_POINT('',(-0.155301544039396,3.40835545433876E-5,1.94940562256037));
#9117=CARTESIAN_POINT('',(-0.15555,4.36677073508985E-14,-0.129405622560373));
#9118=CARTESIAN_POINT('Ctrl Pts',(-0.155681301642334,0.000117756784957245,
1.93559437743963));
#9119=CARTESIAN_POINT('Ctrl Pts',(-0.15531096153354,-0.0438952136125864,
1.93875450306336));
#9120=CARTESIAN_POINT('Ctrl Pts',(-0.112797922286424,-0.14013444255714,
1.94561953298102));
#9121=CARTESIAN_POINT('Ctrl Pts',(0.050423690301781,-0.176807537454614,
1.95618946719261));
#9122=CARTESIAN_POINT('Ctrl Pts',(0.175897409028035,-0.0535121980639788,
1.96730418007439));
#9123=CARTESIAN_POINT('Ctrl Pts',(0.140345725058553,0.118770919429821,1.97841889295616));
#9124=CARTESIAN_POINT('Ctrl Pts',(-0.0236855483435345,0.18232511797358,
1.98953360583794));
#9125=CARTESIAN_POINT('Ctrl Pts',(-0.139699479868363,0.0980903868046811,
1.99859210066576));
#9126=CARTESIAN_POINT('Ctrl Pts',(-0.155368716514435,0.0231492311299511,
2.00394569119965));
#9127=CARTESIAN_POINT('Ctrl Pts',(-0.155307392249976,4.60776613016665E-5,
2.00559437743963));
#9128=CARTESIAN_POINT('Ctrl Pts',(-0.155301544039396,3.40835545433651E-5,
1.94940562256037));
#9129=CARTESIAN_POINT('Ctrl Pts',(-0.15524657988075,-0.0280220748157516,
1.95140757661656));
#9130=CARTESIAN_POINT('Ctrl Pts',(-0.134566760203235,-0.108075727829195,
1.95711443496668));
#9131=CARTESIAN_POINT('Ctrl Pts',(-0.0062604319656806,-0.183750542760931,
1.96652619761073));
#9132=CARTESIAN_POINT('Ctrl Pts',(0.150992567850975,-0.10490328606436,1.9776409104925));
#9133=CARTESIAN_POINT('Ctrl Pts',(0.170019318761453,0.0699777551885857,
1.98875562337428));
#9134=CARTESIAN_POINT('Ctrl Pts',(0.0334017687074566,0.180797612872902,
1.99987033625606));
#9135=CARTESIAN_POINT('Ctrl Pts',(-0.120284414958466,0.1305251314669,2.01008700265142));
#9136=CARTESIAN_POINT('Ctrl Pts',(-0.155177745419853,0.0390452773417597,
2.01659876475286));
#9137=CARTESIAN_POINT('Ctrl Pts',(-0.155535029491756,-0.000142310086639015,
2.01940562256037));
#9138=CARTESIAN_POINT('Origin',(0.,0.,-0.129405622560373));
#9139=CARTESIAN_POINT('',(-0.155675768969518,-0.000119712528699469,1.86559437743963));
#9140=CARTESIAN_POINT('',(-0.15566006707393,0.000124743603163675,1.87940562256037));
#9141=CARTESIAN_POINT('',(-0.15555,4.36677073508985E-14,-0.129405622560373));
#9142=CARTESIAN_POINT('Ctrl Pts',(-0.155675768969518,-0.000119712528699489,
1.86559437743963));
#9143=CARTESIAN_POINT('Ctrl Pts',(-0.155742030728685,-0.00790775711175682,
1.86615350633922));
#9144=CARTESIAN_POINT('Ctrl Pts',(-0.151670179225866,-0.0672314883108279,
1.87041753953273));
#9145=CARTESIAN_POINT('Ctrl Pts',(-0.0754025780794165,-0.16768394396421,
1.87838647702017));
#9146=CARTESIAN_POINT('Ctrl Pts',(0.0999993571785868,-0.154284096420481,
1.88950118990195));
#9147=CARTESIAN_POINT('Ctrl Pts',(0.183856812913126,0.000355232096483363,
1.90061590278373));
#9148=CARTESIAN_POINT('Ctrl Pts',(0.0994024242533403,0.154669363149183,
1.9117306156655));
#9149=CARTESIAN_POINT('Ctrl Pts',(-0.0760499812776094,0.167391320539895,
1.92284532854728));
#9150=CARTESIAN_POINT('Ctrl Pts',(-0.151792203072743,0.0668263219655577,
1.93079991580532));
#9151=CARTESIAN_POINT('Ctrl Pts',(-0.155745145114401,0.00770521701255957,
1.93504959876944));
#9152=CARTESIAN_POINT('Ctrl Pts',(-0.155681301642334,0.000117756784957245,
1.93559437743963));
#9153=CARTESIAN_POINT('Ctrl Pts',(-0.15566006707393,0.000124743603163675,
1.87940562256037));
#9154=CARTESIAN_POINT('Ctrl Pts',(-0.155281954023804,-0.0431477977495249,
1.88251148418635));
#9155=CARTESIAN_POINT('Ctrl Pts',(-0.113998370735902,-0.138671816632529,
1.88932225010624));
#9156=CARTESIAN_POINT('Ctrl Pts',(0.0478348573047686,-0.177525438740387,
1.89983792032007));
#9157=CARTESIAN_POINT('Ctrl Pts',(0.175096732074868,-0.0560766385408066,
1.91095263320185));
#9158=CARTESIAN_POINT('Ctrl Pts',(0.142066184410422,0.116707558540133,1.92206734608362));
#9159=CARTESIAN_POINT('Ctrl Pts',(-0.0210189483701118,0.182651741800479,
1.9331820589654));
#9160=CARTESIAN_POINT('Ctrl Pts',(-0.138953574109165,0.099626766247391,
1.94229481779098));
#9161=CARTESIAN_POINT('Ctrl Pts',(-0.15534829897203,0.0238998867774751,
1.94770267232264));
#9162=CARTESIAN_POINT('Ctrl Pts',(-0.155301544039396,3.40835545433651E-5,
1.94940562256037));
#9163=CARTESIAN_POINT('Origin',(0.,0.,-0.129405622560373));
#9164=CARTESIAN_POINT('',(-0.155305673965381,-4.29356672906584E-5,1.79559437743963));
#9165=CARTESIAN_POINT('',(-0.155696332526243,-0.000111918222169591,1.80940562256037));
#9166=CARTESIAN_POINT('',(-0.15555,4.36677073508985E-14,-0.129405622560373));
#9167=CARTESIAN_POINT('Ctrl Pts',(-0.155305673965381,-4.29356672906715E-5,
1.79559437743963));
#9168=CARTESIAN_POINT('Ctrl Pts',(-0.15536327786609,-0.0233478236154843,
1.797257413909));
#9169=CARTESIAN_POINT('Ctrl Pts',(-0.139503695394343,-0.0984967514743806,
1.80262535467229));
#9170=CARTESIAN_POINT('Ctrl Pts',(-0.0229808287568944,-0.182415282676811,
1.81169819972952));
#9171=CARTESIAN_POINT('Ctrl Pts',(0.140803633131985,-0.118227707163963,
1.82281291261129));
#9172=CARTESIAN_POINT('Ctrl Pts',(0.175689313331093,0.0541915032607811,
1.83392762549307));
#9173=CARTESIAN_POINT('Ctrl Pts',(0.0497400921817236,0.177001065178062,
1.84504233837485));
#9174=CARTESIAN_POINT('Ctrl Pts',(-0.113117186070765,0.139748166323907,
1.85559792235703));
#9175=CARTESIAN_POINT('Ctrl Pts',(-0.155302966541089,0.0436974449055495,
1.86244860204529));
#9176=CARTESIAN_POINT('Ctrl Pts',(-0.155675768969518,-0.000119712528699489,
1.86559437743963));
#9177=CARTESIAN_POINT('Ctrl Pts',(-0.155696332526243,-0.000111918222169581,
1.80940562256037));
#9178=CARTESIAN_POINT('Ctrl Pts',(-0.155753426825624,-0.00714170684078856,
1.8099104874622));
#9179=CARTESIAN_POINT('Ctrl Pts',(-0.15212706396067,-0.0656996999979794,
1.81412025665796));
#9180=CARTESIAN_POINT('Ctrl Pts',(-0.0778446696726029,-0.16656428902048,
1.82203493014764));
#9181=CARTESIAN_POINT('Ctrl Pts',(0.0977343372718058,-0.155728784402163,
1.83314964302942));
#9182=CARTESIAN_POINT('Ctrl Pts',(0.183842378706508,-0.00233125821546848,
1.84426435591119));
#9183=CARTESIAN_POINT('Ctrl Pts',(0.101651789551148,0.15320041988971,1.85537906879297));
#9184=CARTESIAN_POINT('Ctrl Pts',(-0.0735959994667044,0.168484669438591,
1.86649378167474));
#9185=CARTESIAN_POINT('Ctrl Pts',(-0.151326219056215,0.0683587206479964,
1.87450263293055));
#9186=CARTESIAN_POINT('Ctrl Pts',(-0.155732995580608,0.00847092953884112,
1.87880657989242));
#9187=CARTESIAN_POINT('Ctrl Pts',(-0.15566006707393,0.000124743603163675,
1.87940562256037));
#9188=CARTESIAN_POINT('Origin',(0.,0.,-0.129405622560373));
#9189=CARTESIAN_POINT('',(-0.155518343429684,0.000141921497343934,1.72559437743963));
#9190=CARTESIAN_POINT('',(-0.155312812859558,-5.46847567449715E-5,1.73940562256037));
#9191=CARTESIAN_POINT('',(-0.15555,4.36677073508985E-14,-0.129405622560373));
#9192=CARTESIAN_POINT('Ctrl Pts',(-0.155518343429684,0.00014192149734394,
1.72559437743963));
#9193=CARTESIAN_POINT('Ctrl Pts',(-0.155170356887597,-0.0384989847489488,
1.72836132147878));
#9194=CARTESIAN_POINT('Ctrl Pts',(-0.121082051571819,-0.12942764660935,
1.73483316981186));
#9195=CARTESIAN_POINT('Ctrl Pts',(0.0314566718510104,-0.181146160987399,
1.74500992243886));
#9196=CARTESIAN_POINT('Ctrl Pts',(0.169257392597246,-0.071801036869925,
1.75612463532064));
#9197=CARTESIAN_POINT('Ctrl Pts',(0.15211131820417,0.103274395271066,1.76723934820241));
#9198=CARTESIAN_POINT('Ctrl Pts',(-0.00428516586664415,0.18380721203998,
1.77835406108419));
#9199=CARTESIAN_POINT('Ctrl Pts',(-0.133944959179947,0.109200715226807,
1.78780573749659));
#9200=CARTESIAN_POINT('Ctrl Pts',(-0.155234948185403,0.0285706887075647,
1.79355250961507));
#9201=CARTESIAN_POINT('Ctrl Pts',(-0.155305673965381,-4.29356672906715E-5,
1.79559437743963));
#9202=CARTESIAN_POINT('Ctrl Pts',(-0.155312812859558,-5.46847567449889E-5,
1.73940562256037));
#9203=CARTESIAN_POINT('Ctrl Pts',(-0.155383971417563,-0.0225965602306028,
1.74101439503198));
#9204=CARTESIAN_POINT('Ctrl Pts',(-0.140238499174836,-0.0969598979476685,
1.74632807179752));
#9205=CARTESIAN_POINT('Ctrl Pts',(-0.025643765052489,-0.182060023858252,
1.75534665285698));
#9206=CARTESIAN_POINT('Ctrl Pts',(0.139061101343075,-0.120272461796479,
1.76646136573876));
#9207=CARTESIAN_POINT('Ctrl Pts',(0.176462387959855,0.0516186071958565,
1.77757607862053));
#9208=CARTESIAN_POINT('Ctrl Pts',(0.0523210615336027,0.176255387132795,
1.78869079150231));
#9209=CARTESIAN_POINT('Ctrl Pts',(-0.111903083287874,0.141206823406311,
1.79930063948226));
#9210=CARTESIAN_POINT('Ctrl Pts',(-0.155334445600806,0.0444457454539616,
1.80620558316828));
#9211=CARTESIAN_POINT('Ctrl Pts',(-0.155696332526243,-0.000111918222169581,
1.80940562256037));
#9212=CARTESIAN_POINT('Origin',(0.,0.,-0.129405622560373));
#9213=CARTESIAN_POINT('',(-0.155791073984785,-4.23332785624109E-5,1.65559437743963));
#9214=CARTESIAN_POINT('',(-0.15549602743488,0.000140380679560979,1.66940562256037));
#9215=CARTESIAN_POINT('',(-0.15555,4.36677073508985E-14,-0.129405622560373));
#9216=CARTESIAN_POINT('Ctrl Pts',(-0.155791073984785,-4.23332785623931E-5,
1.65559437743963));
#9217=CARTESIAN_POINT('Ctrl Pts',(-0.155799432443742,-0.00234929814144918,
1.65576032475464));
#9218=CARTESIAN_POINT('Ctrl Pts',(-0.154707626121287,-0.056152981769663,
1.65963117636357));
#9219=CARTESIAN_POINT('Ctrl Pts',(-0.0927008570553628,-0.158776588153342,
1.66720693226643));
#9220=CARTESIAN_POINT('Ctrl Pts',(0.0831349670626055,-0.163987899236237,
1.6783216451482));
#9221=CARTESIAN_POINT('Ctrl Pts',(0.182864829055688,-0.0190763764601355,
1.68943635802998));
#9222=CARTESIAN_POINT('Ctrl Pts',(0.115190958951233,0.143298628117334,1.70055107091176));
#9223=CARTESIAN_POINT('Ctrl Pts',(-0.0579345528489473,0.174490806149227,
1.71166578379353));
#9224=CARTESIAN_POINT('Ctrl Pts',(-0.148128299703662,0.0779459344043742,
1.72001355263616));
#9225=CARTESIAN_POINT('Ctrl Pts',(-0.15563630661978,0.0132407170474581,
1.72465641718486));
#9226=CARTESIAN_POINT('Ctrl Pts',(-0.155518343429684,0.00014192149734394,
1.72559437743963));
#9227=CARTESIAN_POINT('Ctrl Pts',(-0.15549602743488,0.000140380679560978,
1.66940562256037));
#9228=CARTESIAN_POINT('Ctrl Pts',(-0.155162551505327,-0.0377565590374548,
1.67211830260176));
#9229=CARTESIAN_POINT('Ctrl Pts',(-0.122151036079771,-0.127932248494189,
1.67853588693708));
#9230=CARTESIAN_POINT('Ctrl Pts',(0.0288064689070301,-0.181586459634089,
1.68865837556633));
#9231=CARTESIAN_POINT('Ctrl Pts',(0.168190194183902,-0.0742665035780993,
1.6997730884481));
#9232=CARTESIAN_POINT('Ctrl Pts',(0.153604091834597,0.101040773675795,1.71088780132988));
#9233=CARTESIAN_POINT('Ctrl Pts',(-0.00159898082742857,0.183850205965748,
1.72200251421165));
#9234=CARTESIAN_POINT('Ctrl Pts',(-0.133085641205322,0.110728808415752,
1.73150845462182));
#9235=CARTESIAN_POINT('Ctrl Pts',(-0.155220097624497,0.0293159959014319,
1.73730949073806));
#9236=CARTESIAN_POINT('Ctrl Pts',(-0.155312812859558,-5.46847567449889E-5,
1.73940562256037));
#9237=CARTESIAN_POINT('Origin',(0.,0.,-0.129405622560373));
#9238=CARTESIAN_POINT('',(-0.155393652545721,-0.000115483920557439,1.58559437743963));
#9239=CARTESIAN_POINT('',(-0.155798596181036,-2.87742873198993E-5,1.59940562256037));
#9240=CARTESIAN_POINT('',(-0.15555,4.36677073508985E-14,-0.129405622560373));
#9241=CARTESIAN_POINT('Ctrl Pts',(-0.155393652545721,-0.000115483920557415,
1.58559437743963));
#9242=CARTESIAN_POINT('Ctrl Pts',(-0.15551609710512,-0.0178853001538728,
1.58686423232442));
#9243=CARTESIAN_POINT('Ctrl Pts',(-0.144494420494594,-0.0873527113820494,
1.59183899150313));
#9244=CARTESIAN_POINT('Ctrl Pts',(-0.042129426749787,-0.178965262680077,
1.60051865497577));
#9245=CARTESIAN_POINT('Ctrl Pts',(0.127521122443655,-0.132445525311824,
1.61163336785754));
#9246=CARTESIAN_POINT('Ctrl Pts',(0.180432373388368,0.0353215582591597,
1.62274808073932));
#9247=CARTESIAN_POINT('Ctrl Pts',(0.0681666854301347,0.170753497304986,
1.6338627936211));
#9248=CARTESIAN_POINT('Ctrl Pts',(-0.103894360880775,0.150180844959855,
1.64481155918787));
#9249=CARTESIAN_POINT('Ctrl Pts',(-0.155612823275166,0.0491555064169759,
1.65205542046071));
#9250=CARTESIAN_POINT('Ctrl Pts',(-0.155791073984785,-4.23332785623931E-5,
1.65559437743963));
#9251=CARTESIAN_POINT('Ctrl Pts',(-0.155798596181035,-2.8774287319909E-5,
1.59940562256037));
#9252=CARTESIAN_POINT('Ctrl Pts',(-0.155802548454758,-0.00158117186309398,
1.59951730587762));
#9253=CARTESIAN_POINT('Ctrl Pts',(-0.155078243731589,-0.0546279421812704,
1.60333389348879));
#9254=CARTESIAN_POINT('Ctrl Pts',(-0.0950109510297781,-0.157405127482403,
1.61085538539389));
#9255=CARTESIAN_POINT('Ctrl Pts',(0.08072995862503,-0.165185134784385,1.62197009827567));
#9256=CARTESIAN_POINT('Ctrl Pts',(0.18256657276441,-0.0217462981307606,
1.63308481115744));
#9257=CARTESIAN_POINT('Ctrl Pts',(0.117272493730902,0.141600201933013,1.64419952403922));
#9258=CARTESIAN_POINT('Ctrl Pts',(-0.0553787694277143,0.175318700856487,
1.65531423692099));
#9259=CARTESIAN_POINT('Ctrl Pts',(-0.147568974074888,0.0794830657980112,
1.66371626976138));
#9260=CARTESIAN_POINT('Ctrl Pts',(-0.155618003819817,0.0140020459368744,
1.66841339830784));
#9261=CARTESIAN_POINT('Ctrl Pts',(-0.15549602743488,0.000140380679560978,
1.66940562256037));
#9262=CARTESIAN_POINT('Origin',(0.,0.,-0.129405622560373));
#9263=CARTESIAN_POINT('',(-0.155374827277607,0.000106566912644677,1.51559437743963));
#9264=CARTESIAN_POINT('',(-0.155411636004792,-0.000122429372152177,1.52940562256037));
#9265=CARTESIAN_POINT('',(-0.15555,4.36677073508985E-14,-0.129405622560373));
#9266=CARTESIAN_POINT('Ctrl Pts',(-0.155374827277607,0.000106566912644665,
1.51559437743963));
#9267=CARTESIAN_POINT('Ctrl Pts',(-0.15516525123262,-0.0331209874429721,
1.5179681398942));
#9268=CARTESIAN_POINT('Ctrl Pts',(-0.128432482276088,-0.118516965374693,
1.52404680664269));
#9269=CARTESIAN_POINT('Ctrl Pts',(0.0121373640243727,-0.183456093490935,
1.53383037768511));
#9270=CARTESIAN_POINT('Ctrl Pts',(0.160721829762796,-0.0892857619226799,
1.54494509056689));
#9271=CARTESIAN_POINT('Ctrl Pts',(0.162173387162441,0.0866212811073344,
1.55605980344866));
#9272=CARTESIAN_POINT('Ctrl Pts',(0.0151632070148183,0.183230813449705,
1.56717451633044));
#9273=CARTESIAN_POINT('Ctrl Pts',(-0.127346320131558,0.120228081953846,
1.57701937432743));
#9274=CARTESIAN_POINT('Ctrl Pts',(-0.155158855203452,0.0339595753935086,
1.58315932803049));
#9275=CARTESIAN_POINT('Ctrl Pts',(-0.155393652545721,-0.000115483920557415,
1.58559437743963));
#9276=CARTESIAN_POINT('Ctrl Pts',(-0.155411636004792,-0.000122429372152195,
1.52940562256037));
#9277=CARTESIAN_POINT('Ctrl Pts',(-0.155536856521019,-0.017127942381014,
1.5306212134474));
#9278=CARTESIAN_POINT('Ctrl Pts',(-0.145123830999224,-0.0858141230320717,
1.53554170862835));
#9279=CARTESIAN_POINT('Ctrl Pts',(-0.0447399086353324,-0.178330579398589,
1.54416710810323));
#9280=CARTESIAN_POINT('Ctrl Pts',(0.125572262560343,-0.134294682876169,
1.55528182098501));
#9281=CARTESIAN_POINT('Ctrl Pts',(0.180929220612589,0.0326813723985916,
1.56639653386679));
#9282=CARTESIAN_POINT('Ctrl Pts',(0.0706544006326465,0.16973924308944,1.57751124674856));
#9283=CARTESIAN_POINT('Ctrl Pts',(-0.102543043975465,0.151593392893447,
1.58851427631309));
#9284=CARTESIAN_POINT('Ctrl Pts',(-0.155671438489139,0.0499169801086266,
1.59581240158369));
#9285=CARTESIAN_POINT('Ctrl Pts',(-0.155798596181035,-2.8774287319909E-5,
1.59940562256037));
#9286=CARTESIAN_POINT('Origin',(0.,0.,-0.129405622560373));
#9287=CARTESIAN_POINT('',(-0.155779565525168,5.70752760268494E-5,1.44559437743963));
#9288=CARTESIAN_POINT('',(-0.155359588126868,9.7796359098748E-5,1.45940562256037));
#9289=CARTESIAN_POINT('',(-0.15555,4.36677073508985E-14,-0.129405622560373));
#9290=CARTESIAN_POINT('Ctrl Pts',(-0.155779565525168,5.707527602684E-5,
1.44559437743963));
#9291=CARTESIAN_POINT('Ctrl Pts',(-0.155551472791767,-0.0482982854834191,
1.44907204746398));
#9292=CARTESIAN_POINT('Ctrl Pts',(-0.105397482190625,-0.148576906771086,
1.45625462178225));
#9293=CARTESIAN_POINT('Ctrl Pts',(0.0653395323085358,-0.171855169727642,
1.46714210039446));
#9294=CARTESIAN_POINT('Ctrl Pts',(0.179824906471596,-0.0382943449728064,
1.47825681327623));
#9295=CARTESIAN_POINT('Ctrl Pts',(0.129689447733715,0.130323063925534,1.48937152615801));
#9296=CARTESIAN_POINT('Ctrl Pts',(-0.0391703041140288,0.179636135340385,
1.50048623903978));
#9297=CARTESIAN_POINT('Ctrl Pts',(-0.143766574204452,0.0890904857756365,
1.50922718946699));
#9298=CARTESIAN_POINT('Ctrl Pts',(-0.155492351860353,0.0187396815013074,
1.51426323560027));
#9299=CARTESIAN_POINT('Ctrl Pts',(-0.155374827277607,0.000106566912644665,
1.51559437743963));
#9300=CARTESIAN_POINT('Ctrl Pts',(-0.155359588126868,9.77963590987375E-5,
1.45940562256037));
#9301=CARTESIAN_POINT('Ctrl Pts',(-0.155172803939685,-0.0323781756248701,
1.46172512101718));
#9302=CARTESIAN_POINT('Ctrl Pts',(-0.129376186277849,-0.116999238532853,
1.46774952376792));
#9303=CARTESIAN_POINT('Ctrl Pts',(0.00945547127077659,-0.183613858508507,
1.47747883081258));
#9304=CARTESIAN_POINT('Ctrl Pts',(0.159400061651521,-0.0916246436218211,
1.48859354369435));
#9305=CARTESIAN_POINT('Ctrl Pts',(0.163421757209686,0.0842424135684204,
1.49970825657613));
#9306=CARTESIAN_POINT('Ctrl Pts',(0.0178388940120074,0.182989695977022,
1.51082296945791));
#9307=CARTESIAN_POINT('Ctrl Pts',(-0.126366486331398,0.121740238415378,
1.52072209145265));
#9308=CARTESIAN_POINT('Ctrl Pts',(-0.155155206713338,0.0347018293285349,
1.52691630915347));
#9309=CARTESIAN_POINT('Ctrl Pts',(-0.155411636004792,-0.000122429372152195,
1.52940562256037));
#9310=CARTESIAN_POINT('Origin',(0.,0.,-0.129405622560373));
#9311=CARTESIAN_POINT('',(-0.155544028068607,-0.000142255349246604,1.37559437743963));
#9312=CARTESIAN_POINT('',(-0.155766970030976,6.94820370851796E-5,1.38940562256037));
#9313=CARTESIAN_POINT('',(-0.15555,4.36677073508985E-14,-0.129405622560373));
#9314=CARTESIAN_POINT('Ctrl Pts',(-0.155544028068607,-0.000142255349246624,
1.37559437743963));
#9315=CARTESIAN_POINT('Ctrl Pts',(-0.155656157486624,-0.0123800086342895,
1.37647105073983));
#9316=CARTESIAN_POINT('Ctrl Pts',(-0.14874404615406,-0.0762104595352229,
1.38105262833397));
#9317=CARTESIAN_POINT('Ctrl Pts',(-0.0608062091124237,-0.173510975957692,
1.38933911022202));
#9318=CARTESIAN_POINT('Ctrl Pts',(0.112810477944863,-0.145180060305354,
1.4004538231038));
#9319=CARTESIAN_POINT('Ctrl Pts',(0.183154736262308,0.0160560402683587,
1.41156853598558));
#9320=CARTESIAN_POINT('Ctrl Pts',(0.0858298667327937,0.162593627861136,
1.42268324886735));
#9321=CARTESIAN_POINT('Ctrl Pts',(-0.0900680126570708,0.160284768273284,
1.43379796174913));
#9322=CARTESIAN_POINT('Ctrl Pts',(-0.154275150059787,0.0578765860113586,
1.44143500460655));
#9323=CARTESIAN_POINT('Ctrl Pts',(-0.155794469321476,0.00321666057460228,
1.44536714317005));
#9324=CARTESIAN_POINT('Ctrl Pts',(-0.155779565525168,5.707527602684E-5,
1.44559437743963));
#9325=CARTESIAN_POINT('Ctrl Pts',(-0.155766970030976,6.94820370851787E-5,
1.38940562256037));
#9326=CARTESIAN_POINT('Ctrl Pts',(-0.155501349034121,-0.047541582630428,
1.39282902858696));
#9327=CARTESIAN_POINT('Ctrl Pts',(-0.106708006897432,-0.147149458313824,
1.39995733890748));
#9328=CARTESIAN_POINT('Ctrl Pts',(0.062821469496632,-0.172791544768887,
1.41079055352192));
#9329=CARTESIAN_POINT('Ctrl Pts',(0.179246168325776,-0.0409177970309031,
1.4219052664037));
#9330=CARTESIAN_POINT('Ctrl Pts',(0.131579840483081,0.12841417582098,1.43301997928547));
#9331=CARTESIAN_POINT('Ctrl Pts',(-0.0365413417972516,0.180189304102632,
1.44413469216725));
#9332=CARTESIAN_POINT('Ctrl Pts',(-0.143106948997553,0.090629082605181,
1.45292990659221));
#9333=CARTESIAN_POINT('Ctrl Pts',(-0.155471151858434,0.0194952661097169,
1.45802021672326));
#9334=CARTESIAN_POINT('Ctrl Pts',(-0.155359588126868,9.77963590987375E-5,
1.45940562256037));
#9335=CARTESIAN_POINT('Origin',(0.,0.,-0.129405622560373));
#9336=CARTESIAN_POINT('',(-0.155299722974107,2.92844383266709E-5,1.30559437743963));
#9337=CARTESIAN_POINT('',(-0.155567011638057,-0.00014128583726751,1.31940562256037));
#9338=CARTESIAN_POINT('',(-0.15555,4.36677073508985E-14,-0.129405622560373));
#9339=CARTESIAN_POINT('Ctrl Pts',(-0.155299722974107,2.92844383266832E-5,
1.30559437743963));
#9340=CARTESIAN_POINT('Ctrl Pts',(-0.155253032879804,-0.0277281524137369,
1.30757495830962));
#9341=CARTESIAN_POINT('Ctrl Pts',(-0.1348961631779,-0.107472984602923,1.31326044347353));
#9342=CARTESIAN_POINT('Ctrl Pts',(-0.00731787249863105,-0.183711465582603,
1.32265083293137));
#9343=CARTESIAN_POINT('Ctrl Pts',(0.150386311950183,-0.10577055839144,1.33376554581314));
#9344=CARTESIAN_POINT('Ctrl Pts',(0.170419244869387,0.0689980783976093,
1.34488025869492));
#9345=CARTESIAN_POINT('Ctrl Pts',(0.0344417641967487,0.180602377402486,
1.35599497157669));
#9346=CARTESIAN_POINT('Ctrl Pts',(-0.119853316330062,0.131111926080083,
1.36623301115827));
#9347=CARTESIAN_POINT('Ctrl Pts',(-0.155182287959412,0.0393378943554936,
1.37276614644591));
#9348=CARTESIAN_POINT('Ctrl Pts',(-0.155544028068607,-0.000142255349246624,
1.37559437743963));
#9349=CARTESIAN_POINT('Ctrl Pts',(-0.155567011638057,-0.000141285837267533,
1.31940562256037));
#9350=CARTESIAN_POINT('Ctrl Pts',(-0.155672941482856,-0.011617212227624,
1.32022803186282));
#9351=CARTESIAN_POINT('Ctrl Pts',(-0.149275241288209,-0.074674446500909,
1.32475534545919));
#9352=CARTESIAN_POINT('Ctrl Pts',(-0.0633350012944175,-0.172603976154579,
1.33298756334949));
#9353=CARTESIAN_POINT('Ctrl Pts',(0.110677115627384,-0.146812911726923,
1.34410227623126));
#9354=CARTESIAN_POINT('Ctrl Pts',(0.183369791793454,0.0133781325662369,
1.35521698911304));
#9355=CARTESIAN_POINT('Ctrl Pts',(0.0881964673803512,0.161322156305205,
1.36633170199482));
#9356=CARTESIAN_POINT('Ctrl Pts',(-0.087716373065073,0.161583702363956,
1.37744641487659));
#9357=CARTESIAN_POINT('Ctrl Pts',(-0.153879808881157,0.0594037195771841,
1.38513772173178));
#9358=CARTESIAN_POINT('Ctrl Pts',(-0.155788811393,0.0039844229192785,1.38912412429304));
#9359=CARTESIAN_POINT('Ctrl Pts',(-0.155766970030976,6.94820370851787E-5,
1.38940562256037));
#9360=CARTESIAN_POINT('Origin',(0.,0.,-0.129405622560373));
#9361=CARTESIAN_POINT('',(-0.155651485174645,0.000127186369725584,1.23559437743963));
#9362=CARTESIAN_POINT('',(-0.155296357294745,1.69605947035745E-5,1.24940562256037));
#9363=CARTESIAN_POINT('',(-0.15555,4.36677073508985E-14,-0.129405622560373));
#9364=CARTESIAN_POINT('Ctrl Pts',(-0.155651485174645,0.00012718636972558,
1.23559437743963));
#9365=CARTESIAN_POINT('Ctrl Pts',(-0.155271426560331,-0.0428537130042785,
1.2386788658794));
#9366=CARTESIAN_POINT('Ctrl Pts',(-0.114466114921002,-0.13809428189611,
1.24546825861309));
#9367=CARTESIAN_POINT('Ctrl Pts',(0.0468123474454561,-0.177797800804905,
1.25596255564071));
#9368=CARTESIAN_POINT('Ctrl Pts',(0.174771089844121,-0.0570834476806803,
1.26707726852248));
#9369=CARTESIAN_POINT('Ctrl Pts',(0.142735519209796,0.115887986436578,1.27819198140426));
#9370=CARTESIAN_POINT('Ctrl Pts',(-0.0199673795378149,0.182769684572709,
1.28930669428604));
#9371=CARTESIAN_POINT('Ctrl Pts',(-0.138655607475008,0.100231705012538,
1.29844082629783));
#9372=CARTESIAN_POINT('Ctrl Pts',(-0.155340372070791,0.0241953254608532,
1.30387005401569));
#9373=CARTESIAN_POINT('Ctrl Pts',(-0.155299722974107,2.92844383266832E-5,
1.30559437743963));
#9374=CARTESIAN_POINT('Ctrl Pts',(-0.155296357294745,1.6960594703571E-5,
1.24940562256037));
#9375=CARTESIAN_POINT('Ctrl Pts',(-0.155270088652903,-0.0269814387089377,
1.2513319394326));
#9376=CARTESIAN_POINT('Ctrl Pts',(-0.135721405315835,-0.105941739255518,
1.25696316059875));
#9377=CARTESIAN_POINT('Ctrl Pts',(-0.0100014200241654,-0.183584930129994,
1.26629928605883));
#9378=CARTESIAN_POINT('Ctrl Pts',(0.148824776878697,-0.107956661491269,
1.2774139989406));
#9379=CARTESIAN_POINT('Ctrl Pts',(0.171409230594902,0.0665006063145147,
1.28852871182238));
#9380=CARTESIAN_POINT('Ctrl Pts',(0.0370769876137034,0.180079848852746,
1.29964342470416));
#9381=CARTESIAN_POINT('Ctrl Pts',(-0.118746306416021,0.132598853125113,
1.30993572828349));
#9382=CARTESIAN_POINT('Ctrl Pts',(-0.155195733922481,0.040081143851182,
1.31652312756889));
#9383=CARTESIAN_POINT('Ctrl Pts',(-0.155567011638057,-0.000141285837267533,
1.31940562256037));
#9384=CARTESIAN_POINT('Origin',(0.,0.,-0.129405622560373));
#9385=CARTESIAN_POINT('',(-0.155704137558009,-0.000108555906714621,1.16559437743963));
#9386=CARTESIAN_POINT('',(-0.155629273963861,0.000132584196566119,1.17940562256037));
#9387=CARTESIAN_POINT('',(-0.15555,4.36677073508985E-14,-0.129405622560373));
#9388=CARTESIAN_POINT('Ctrl Pts',(-0.155704137558009,-0.000108555906714635,
1.16559437743963));
#9389=CARTESIAN_POINT('Ctrl Pts',(-0.155757622145014,-0.00683986061081713,
1.16607786915525));
#9390=CARTESIAN_POINT('Ctrl Pts',(-0.152303640106945,-0.0650965997331611,
1.1702662651648));
#9391=CARTESIAN_POINT('Ctrl Pts',(-0.0788020109327346,-0.166113506125697,
1.17815956546827));
#9392=CARTESIAN_POINT('Ctrl Pts',(0.0968364469996555,-0.156288695614551,
1.18927427835005));
#9393=CARTESIAN_POINT('Ctrl Pts',(0.183825913682498,-0.00338929243493567,
1.20038899123183));
#9394=CARTESIAN_POINT('Ctrl Pts',(0.102531822692703,0.152612840808782,1.2115037041136));
#9395=CARTESIAN_POINT('Ctrl Pts',(-0.0726250950973966,0.168905445165361,
1.22261841699538));
#9396=CARTESIAN_POINT('Ctrl Pts',(-0.151139256233472,0.0689625117337061,
1.23064864143739));
#9397=CARTESIAN_POINT('Ctrl Pts',(-0.155727930392202,0.00877239024010237,
1.23497396158547));
#9398=CARTESIAN_POINT('Ctrl Pts',(-0.155651485174645,0.00012718636972558,
1.23559437743963));
#9399=CARTESIAN_POINT('Ctrl Pts',(-0.155629273963861,0.000132584196566117,
1.17940562256037));
#9400=CARTESIAN_POINT('Ctrl Pts',(-0.155246937989768,-0.0421077654193814,
1.18243584700238));
#9401=CARTESIAN_POINT('Ctrl Pts',(-0.115640831727419,-0.136624465004964,
1.18917097573831));
#9402=CARTESIAN_POINT('Ctrl Pts',(0.0442094305335735,-0.178462828693349,
1.19961100876817));
#9403=CARTESIAN_POINT('Ctrl Pts',(0.173918351244622,-0.0596310495772682,
1.21072572164995));
#9404=CARTESIAN_POINT('Ctrl Pts',(0.144413599053411,0.113790014420313,1.22184043453173));
#9405=CARTESIAN_POINT('Ctrl Pts',(-0.0172946805849302,0.183041932345569,
1.2329551474135));
#9406=CARTESIAN_POINT('Ctrl Pts',(-0.137888448107413,0.101767008220966,
1.24214354342305));
#9407=CARTESIAN_POINT('Ctrl Pts',(-0.155320611391586,0.0249448497181091,
1.24762703513867));
#9408=CARTESIAN_POINT('Ctrl Pts',(-0.155296357294745,1.6960594703571E-5,
1.24940562256037));
#9409=CARTESIAN_POINT('Origin',(0.,0.,-0.129405622560373));
#9410=CARTESIAN_POINT('',(-0.155316093427556,-5.92046854689235E-5,1.09559437743963));
#9411=CARTESIAN_POINT('',(-0.155723105325903,-9.93094234179315E-5,1.10940562256037));
#9412=CARTESIAN_POINT('',(-0.15555,4.36677073508985E-14,-0.129405622560373));
#9413=CARTESIAN_POINT('Ctrl Pts',(-0.155316093427556,-5.92046854689179E-5,
1.09559437743963));
#9414=CARTESIAN_POINT('Ctrl Pts',(-0.155392202162635,-0.0223004273098781,
1.09718177672503));
#9415=CARTESIAN_POINT('Ctrl Pts',(-0.140523796570003,-0.0963544111096822,
1.10247408030436));
#9416=CARTESIAN_POINT('Ctrl Pts',(-0.0266911547466422,-0.181909417300769,
1.11147128817762));
#9417=CARTESIAN_POINT('Ctrl Pts',(0.138366588630194,-0.121070809839768,
1.12258600105939));
#9418=CARTESIAN_POINT('Ctrl Pts',(0.176756544363487,0.0506021528108583,
1.13370071394117));
#9419=CARTESIAN_POINT('Ctrl Pts',(0.053334601374032,0.175951340263971,1.14481542682295));
#9420=CARTESIAN_POINT('Ctrl Pts',(-0.11141976168757,0.141779822134275,1.1554466479891));
#9421=CARTESIAN_POINT('Ctrl Pts',(-0.155347780011936,0.0447408364230817,
1.16237296486133));
#9422=CARTESIAN_POINT('Ctrl Pts',(-0.155704137558009,-0.000108555906714635,
1.16559437743963));
#9423=CARTESIAN_POINT('Ctrl Pts',(-0.155723105325903,-9.93094234179323E-5,
1.10940562256037));
#9424=CARTESIAN_POINT('Ctrl Pts',(-0.155767528832372,-0.00607323109599136,
1.10983485027824));
#9425=CARTESIAN_POINT('Ctrl Pts',(-0.152743452599297,-0.0635660122040492,
1.11396898229003));
#9426=CARTESIAN_POINT('Ctrl Pts',(-0.0812207929765285,-0.164944347467861,
1.12180801859574));
#9427=CARTESIAN_POINT('Ctrl Pts',(0.0945424741868258,-0.15768695427323,
1.13292273147752));
#9428=CARTESIAN_POINT('Ctrl Pts',(0.183756769071919,-0.00607493157030043,
1.14403744435929));
#9429=CARTESIAN_POINT('Ctrl Pts',(0.104750804765144,0.151098391369297,1.15515215724107));
#9430=CARTESIAN_POINT('Ctrl Pts',(-0.0701493549889435,0.169948589190878,
1.16626687012284));
#9431=CARTESIAN_POINT('Ctrl Pts',(-0.150655835862288,0.0704960085261505,
1.17435135856261));
#9432=CARTESIAN_POINT('Ctrl Pts',(-0.155714401116427,0.00953740333429069,
1.17873094270845));
#9433=CARTESIAN_POINT('Ctrl Pts',(-0.155629273963861,0.000132584196566117,
1.17940562256037));
#9434=CARTESIAN_POINT('Origin',(0.,0.,-0.129405622560373));
#9435=CARTESIAN_POINT('',(-0.155487379626493,0.000139458551422749,1.02559437743963));
#9436=CARTESIAN_POINT('',(-0.155325604028858,-7.03580820835548E-5,1.03940562256037));
#9437=CARTESIAN_POINT('',(-0.15555,4.36677073508985E-14,-0.129405622560373));
#9438=CARTESIAN_POINT('Ctrl Pts',(-0.155487379626493,0.000139458551422741,
1.02559437743963));
#9439=CARTESIAN_POINT('Ctrl Pts',(-0.15516015826044,-0.0374642026468413,
1.02828568429481));
#9440=CARTESIAN_POINT('Ctrl Pts',(-0.122567220013461,-0.127342229539981,
1.03468189544392));
#9441=CARTESIAN_POINT('Ctrl Pts',(0.0277609020139879,-0.181749239788739,
1.04478301088696));
#9442=CARTESIAN_POINT('Ctrl Pts',(0.167759977846949,-0.0752332617743367,
1.05589772376874));
#9443=CARTESIAN_POINT('Ctrl Pts',(0.154183067891921,0.10015505688606,1.06701243665051));
#9444=CARTESIAN_POINT('Ctrl Pts',(-0.000540836401177662,0.183856360619919,
1.07812714953229));
#9445=CARTESIAN_POINT('Ctrl Pts',(-0.132742730727165,0.111330221780279,
1.08765446312866));
#9446=CARTESIAN_POINT('Ctrl Pts',(-0.155214568480931,0.0296093864093298,
1.09347687243111));
#9447=CARTESIAN_POINT('Ctrl Pts',(-0.155316093427556,-5.92046854689179E-5,
1.09559437743963));
#9448=CARTESIAN_POINT('Ctrl Pts',(-0.155325604028858,-7.03580820835287E-5,
1.03940562256037));
#9449=CARTESIAN_POINT('Ctrl Pts',(-0.155413268812163,-0.0215479955240541,
1.04093875784802));
#9450=CARTESIAN_POINT('Ctrl Pts',(-0.141237759605696,-0.0948168172565819,
1.04617679742959));
#9451=CARTESIAN_POINT('Ctrl Pts',(-0.0293463034743252,-0.181499998473078,
1.05511974130508));
#9452=CARTESIAN_POINT('Ctrl Pts',(0.136582774532958,-0.123079651747206,
1.06623445418686));
#9453=CARTESIAN_POINT('Ctrl Pts',(0.177477058724911,0.048014045858363,1.07734916706863));
#9454=CARTESIAN_POINT('Ctrl Pts',(0.0558998488320383,0.175153252535857,
1.08846387995041));
#9455=CARTESIAN_POINT('Ctrl Pts',(-0.110179630765451,0.143230603341919,
1.09914936511432));
#9456=CARTESIAN_POINT('Ctrl Pts',(-0.155384084723293,0.0454910252069913,
1.10612994598431));
#9457=CARTESIAN_POINT('Ctrl Pts',(-0.155723105325903,-9.93094234179323E-5,
1.10940562256037));
#9458=CARTESIAN_POINT('Origin',(0.,0.,-0.129405622560373));
#9459=CARTESIAN_POINT('',(-0.155800812044169,-2.33349500279874E-5,0.955594377439629));
#9460=CARTESIAN_POINT('',(-0.155465886400055,0.000136334869802884,0.969405622560371));
#9461=CARTESIAN_POINT('',(-0.15555,4.36677073508985E-14,-0.129405622560373));
#9462=CARTESIAN_POINT('Ctrl Pts',(-0.155800812044169,-2.33349500279754E-5,
0.955594377439629));
#9463=CARTESIAN_POINT('Ctrl Pts',(-0.155803439542059,-0.00127859733407187,
0.95568468757067));
#9464=CARTESIAN_POINT('Ctrl Pts',(-0.155221069917255,-0.0540275413746436,
0.959479901995636));
#9465=CARTESIAN_POINT('Ctrl Pts',(-0.0959152937319705,-0.156855698885072,
0.966980020714528));
#9466=CARTESIAN_POINT('Ctrl Pts',(0.0797779258821927,-0.165647023475673,
0.978094733596302));
#9467=CARTESIAN_POINT('Ctrl Pts',(0.182438389002691,-0.0227966677941671,
0.989209446478081));
#9468=CARTESIAN_POINT('Ctrl Pts',(0.118085504862125,0.140922912920049,1.00032415935986));
#9469=CARTESIAN_POINT('Ctrl Pts',(-0.0543688349964322,0.175634517181406,
1.01143887224163));
#9470=CARTESIAN_POINT('Ctrl Pts',(-0.147344990269918,0.0800886216370419,
1.01986227826822));
#9471=CARTESIAN_POINT('Ctrl Pts',(-0.15561061742745,0.0143017138157724,
1.02458078000089));
#9472=CARTESIAN_POINT('Ctrl Pts',(-0.155487379626493,0.000139458551422741,
1.02559437743963));
#9473=CARTESIAN_POINT('Ctrl Pts',(-0.155465886400055,0.000136334869802876,
0.969405622560371));
#9474=CARTESIAN_POINT('Ctrl Pts',(-0.15515576719121,-0.0367220611351339,
0.972042665417797));
#9475=CARTESIAN_POINT('Ctrl Pts',(-0.123611600275362,-0.125841774747843,
0.978384612569147));
#9476=CARTESIAN_POINT('Ctrl Pts',(0.0251022815740214,-0.182135472747933,
0.988431464014426));
#9477=CARTESIAN_POINT('Ctrl Pts',(0.166642788778922,-0.0776764824211173,
0.999546176896201));
#9478=CARTESIAN_POINT('Ctrl Pts',(0.155630041687788,0.0978914965540504,
1.01066088977798));
#9479=CARTESIAN_POINT('Ctrl Pts',(0.00214566711329121,0.183844638447722,
1.02177560265976));
#9480=CARTESIAN_POINT('Ctrl Pts',(-0.131860770774095,0.112855894150209,
1.03135718025388));
#9481=CARTESIAN_POINT('Ctrl Pts',(-0.155201422124717,0.0303538762959815,
1.03723385355409));
#9482=CARTESIAN_POINT('Ctrl Pts',(-0.155325604028858,-7.03580820835287E-5,
1.03940562256037));
#9483=CARTESIAN_POINT('Origin',(0.,0.,-0.129405622560373));
#9484=CARTESIAN_POINT('',(-0.155419028575706,-0.000124905745103449,0.885594377439629));
#9485=CARTESIAN_POINT('',(-0.155804426663874,-9.35735450183217E-6,0.899405622560371));
#9486=CARTESIAN_POINT('',(-0.15555,4.36677073508985E-14,-0.129405622560373));
#9487=CARTESIAN_POINT('Ctrl Pts',(-0.155419028575706,-0.000124905745103449,
0.885594377439629));
#9488=CARTESIAN_POINT('Ctrl Pts',(-0.155544942580047,-0.0168294139448893,
0.88678859514045));
#9489=CARTESIAN_POINT('Ctrl Pts',(-0.145367891922091,-0.0852081429960637,
0.891687717135198));
#9490=CARTESIAN_POINT('Ctrl Pts',(-0.0457655175701415,-0.178070130134034,
0.90029174342387));
#9491=CARTESIAN_POINT('Ctrl Pts',(0.124797271018106,-0.135015165780915,
0.911406456305646));
#9492=CARTESIAN_POINT('Ctrl Pts',(0.18111431299722,0.0316395238895826,0.922521169187422));
#9493=CARTESIAN_POINT('Ctrl Pts',(0.071630133994783,0.169329789902144,0.933635882069198));
#9494=CARTESIAN_POINT('Ctrl Pts',(-0.102005504702542,0.152147737220529,
0.944660284819935));
#9495=CARTESIAN_POINT('Ctrl Pts',(-0.15569564844375,0.0502175852432928,
0.951979783276744));
#9496=CARTESIAN_POINT('Ctrl Pts',(-0.155800812044169,-2.33349500279754E-5,
0.955594377439629));
#9497=CARTESIAN_POINT('Ctrl Pts',(-0.155804426663874,-9.35735450181938E-6,
0.899405622560371));
#9498=CARTESIAN_POINT('Ctrl Pts',(-0.155804862851121,-0.000510348018169845,
0.899441668693652));
#9499=CARTESIAN_POINT('Ctrl Pts',(-0.155575767654156,-0.0525038984009843,
0.90318261912086));
#9500=CARTESIAN_POINT('Ctrl Pts',(-0.0981969772278097,-0.155437475007334,
0.910628473841992));
#9501=CARTESIAN_POINT('Ctrl Pts',(0.0773490332209564,-0.16679503000125,
0.921743186723768));
#9502=CARTESIAN_POINT('Ctrl Pts',(0.182085818614306,-0.0254599613686364,
0.932857899605545));
#9503=CARTESIAN_POINT('Ctrl Pts',(0.120132017548368,0.139182446210336,0.943972612487321));
#9504=CARTESIAN_POINT('Ctrl Pts',(-0.0517967206657041,0.176410188769281,
0.955087325369096));
#9505=CARTESIAN_POINT('Ctrl Pts',(-0.146766922130325,0.0816263333357911,
0.963564995393448));
#9506=CARTESIAN_POINT('Ctrl Pts',(-0.155591468107198,0.0150620155784236,
0.968337761123872));
#9507=CARTESIAN_POINT('Ctrl Pts',(-0.155465886400055,0.000136334869802876,
0.969405622560371));
#9508=CARTESIAN_POINT('Origin',(0.,0.,-0.129405622560373));
#9509=CARTESIAN_POINT('',(-0.155353971596541,9.41326338506563E-5,0.815594377439629));
#9510=CARTESIAN_POINT('',(-0.15543853527939,-0.000130502868957535,0.829405622560371));
#9511=CARTESIAN_POINT('',(-0.15555,4.36677073508985E-14,-0.129405622560373));
#9512=CARTESIAN_POINT('Ctrl Pts',(-0.155353971596541,9.41326338506562E-5,
0.815594377439629));
#9513=CARTESIAN_POINT('Ctrl Pts',(-0.155176235752476,-0.0320855025530675,
0.817892502710232));
#9514=CARTESIAN_POINT('Ctrl Pts',(-0.129743274287226,-0.116400787456992,
0.823895532274761));
#9515=CARTESIAN_POINT('Ctrl Pts',(0.00839855685065273,-0.18366523374673,
0.833603466133212));
#9516=CARTESIAN_POINT('Ctrl Pts',(0.158870089284654,-0.0925405239616719,
0.844718179014991));
#9517=CARTESIAN_POINT('Ctrl Pts',(0.163903890459678,0.0833004714068091,
0.855832891896764));
#9518=CARTESIAN_POINT('Ctrl Pts',(0.0188917636673275,0.182883993585968,
0.866947604778543));
#9519=CARTESIAN_POINT('Ctrl Pts',(-0.125975846208109,0.122335050954643,
0.876868099959496));
#9520=CARTESIAN_POINT('Ctrl Pts',(-0.15515431084261,0.0349941389255136,
0.883083690846525));
#9521=CARTESIAN_POINT('Ctrl Pts',(-0.155419028575706,-0.000124905745103449,
0.885594377439629));
#9522=CARTESIAN_POINT('Ctrl Pts',(-0.15543853527939,-0.000130502868957542,
0.82940562256037));
#9523=CARTESIAN_POINT('Ctrl Pts',(-0.155565218715822,-0.0160709251164858,
0.830545576263433));
#9524=CARTESIAN_POINT('Ctrl Pts',(-0.145977858350589,-0.0836697618712271,
0.835390434260421));
#9525=CARTESIAN_POINT('Ctrl Pts',(-0.0483625319738309,-0.177382413092208,
0.843940196551336));
#9526=CARTESIAN_POINT('Ctrl Pts',(0.122811155175551,-0.136824249085392,
0.855054909433111));
#9527=CARTESIAN_POINT('Ctrl Pts',(0.18155728681432,0.0289897667799704,0.866169622314888));
#9528=CARTESIAN_POINT('Ctrl Pts',(0.0740966767894734,0.168265080935085,
0.877284335196663));
#9529=CARTESIAN_POINT('Ctrl Pts',(-0.100627295271696,0.153549890455044,
0.888363001945158));
#9530=CARTESIAN_POINT('Ctrl Pts',(-0.155760030525013,0.0509826220191848,
0.895736764399727));
#9531=CARTESIAN_POINT('Ctrl Pts',(-0.155804426663874,-9.35735450181938E-6,
0.899405622560371));
#9532=CARTESIAN_POINT('Origin',(0.,0.,-0.129405622560373));
#9533=CARTESIAN_POINT('',(-0.155761438252094,7.41758372851551E-5,0.74559437743963));
#9534=CARTESIAN_POINT('',(-0.155340757131295,8.43414871359027E-5,0.759405622560371));
#9535=CARTESIAN_POINT('',(-0.15555,4.36677073508985E-14,-0.129405622560373));
#9536=CARTESIAN_POINT('Ctrl Pts',(-0.155761438252094,7.41758372851484E-5,
0.74559437743963));
#9537=CARTESIAN_POINT('Ctrl Pts',(-0.155482663215916,-0.0472440860383338,
0.748996410280013));
#9538=CARTESIAN_POINT('Ctrl Pts',(-0.107218957683579,-0.146585393585093,
0.756103347414322));
#9539=CARTESIAN_POINT('Ctrl Pts',(0.0618259562826469,-0.173150238157939,
0.766915188842555));
#9540=CARTESIAN_POINT('Ctrl Pts',(0.179007701381185,-0.0419487388444433,
0.778029901724333));
#9541=CARTESIAN_POINT('Ctrl Pts',(0.132316724534454,0.127654761967143,0.789144614606108));
#9542=CARTESIAN_POINT('Ctrl Pts',(-0.0355036877557856,0.180396624137356,
0.800259327487885));
#9543=CARTESIAN_POINT('Ctrl Pts',(-0.142843189124192,0.0912350616645566,
0.809075915099058));
#9544=CARTESIAN_POINT('Ctrl Pts',(-0.155462771173448,0.0197926392114622,
0.814187598416307));
#9545=CARTESIAN_POINT('Ctrl Pts',(-0.155353971596541,9.41326338506562E-5,
0.815594377439629));
#9546=CARTESIAN_POINT('Ctrl Pts',(-0.155340757131295,8.43414871358941E-5,
0.759405622560371));
#9547=CARTESIAN_POINT('Ctrl Pts',(-0.155186065178493,-0.0313421581146853,
0.761649483833214));
#9548=CARTESIAN_POINT('Ctrl Pts',(-0.130663644838326,-0.114879826414827,
0.767598249399983));
#9549=CARTESIAN_POINT('Ctrl Pts',(0.0057140072891202,-0.183768346278771,
0.777251919260679));
#9550=CARTESIAN_POINT('Ctrl Pts',(0.157500961365389,-0.0948520012562343,
0.788366632142453));
#9551=CARTESIAN_POINT('Ctrl Pts',(0.165103553267307,0.080896672810716,0.799481345024232));
#9552=CARTESIAN_POINT('Ctrl Pts',(0.0215619850688987,0.182588432747595,
0.810596057906006));
#9553=CARTESIAN_POINT('Ctrl Pts',(-0.124972046377392,0.123843126491084,
0.820570817084721));
#9554=CARTESIAN_POINT('Ctrl Pts',(-0.155153491462033,0.0357362129042795,
0.826840671969508));
#9555=CARTESIAN_POINT('Ctrl Pts',(-0.15543853527939,-0.000130502868957542,
0.82940562256037));
#9556=CARTESIAN_POINT('Origin',(0.,0.,-0.129405622560373));
#9557=CARTESIAN_POINT('',(-0.155576082774588,-0.000140575406353809,0.675594377439629));
#9558=CARTESIAN_POINT('',(-0.155746091141148,8.55458678441536E-5,0.689405622560371));
#9559=CARTESIAN_POINT('',(-0.15555,4.36677073508985E-14,-0.129405622560373));
#9560=CARTESIAN_POINT('Ctrl Pts',(-0.155576082774588,-0.000140575406353826,
0.675594377439629));
#9561=CARTESIAN_POINT('Ctrl Pts',(-0.15567933078646,-0.0113165881608609,
0.676395413555869));
#9562=CARTESIAN_POINT('Ctrl Pts',(-0.149480883924574,-0.0740696137198915,
0.680901353966033));
#9563=CARTESIAN_POINT('Ctrl Pts',(-0.0643273434762849,-0.172236601004835,
0.689112198670122));
#9564=CARTESIAN_POINT('Ctrl Pts',(0.10983032453655,-0.147447460665183,0.7002269115519));
#9565=CARTESIAN_POINT('Ctrl Pts',(0.183443747273531,0.0123225577969614,
0.711341624433675));
#9566=CARTESIAN_POINT('Ctrl Pts',(0.0891234668368183,0.160811882345183,
0.722456337315452));
#9567=CARTESIAN_POINT('Ctrl Pts',(-0.0867849519149494,0.162085859856851,
0.733571050197227));
#9568=CARTESIAN_POINT('Ctrl Pts',(-0.153720861082027,0.0600054806471056,
0.74128373023862));
#9569=CARTESIAN_POINT('Ctrl Pts',(-0.155786256648735,0.00428676032007601,
0.745291505986088));
#9570=CARTESIAN_POINT('Ctrl Pts',(-0.155761438252094,7.41758372851484E-5,
0.74559437743963));
#9571=CARTESIAN_POINT('Ctrl Pts',(-0.155746091141148,8.5545867844157E-5,
0.689405622560371));
#9572=CARTESIAN_POINT('Ctrl Pts',(-0.155437871285066,-0.0464900844783075,
0.692753391402996));
#9573=CARTESIAN_POINT('Ctrl Pts',(-0.108502980662635,-0.145148810790092,
0.699806064539545));
#9574=CARTESIAN_POINT('Ctrl Pts',(0.0592893454135225,-0.174035135802431,
0.710563641970021));
#9575=CARTESIAN_POINT('Ctrl Pts',(0.17837565371923,-0.0445598601161589,
0.721678354851797));
#9576=CARTESIAN_POINT('Ctrl Pts',(0.134167848541566,0.125707769811822,0.732793067733573));
#9577=CARTESIAN_POINT('Ctrl Pts',(-0.0328640048105861,0.18089613639087,
0.743907780615349));
#9578=CARTESIAN_POINT('Ctrl Pts',(-0.142163443840071,0.0927734423224093,
0.752778632224282));
#9579=CARTESIAN_POINT('Ctrl Pts',(-0.15544148153917,0.0205470449866602,
0.757944579539289));
#9580=CARTESIAN_POINT('Ctrl Pts',(-0.155340757131295,8.43414871358941E-5,
0.759405622560371));
#9581=CARTESIAN_POINT('Origin',(0.,0.,-0.129405622560373));
#9582=CARTESIAN_POINT('',(-0.155295522970368,1.20667024935662E-5,0.605594377439629));
#9583=CARTESIAN_POINT('',(-0.155599079595997,-0.000137936170561209,0.61940562256037));
#9584=CARTESIAN_POINT('',(-0.15555,4.36677073508985E-14,-0.129405622560373));
#9585=CARTESIAN_POINT('Ctrl Pts',(-0.155295522970368,1.20667024935545E-5,
0.605594377439629));
#9586=CARTESIAN_POINT('Ctrl Pts',(-0.155277046884744,-0.0266871317790742,
0.607499321125649));
#9587=CARTESIAN_POINT('Ctrl Pts',(-0.136042101589265,-0.105338263915341,
0.613109169105595));
#9588=CARTESIAN_POINT('Ctrl Pts',(-0.0110578453815636,-0.183524325090524,
0.622423921379466));
#9589=CARTESIAN_POINT('Ctrl Pts',(0.148200983745356,-0.108811406852975,
0.633538634261242));
#9590=CARTESIAN_POINT('Ctrl Pts',(0.171789121533681,0.0655129877741882,
0.644653347143018));
#9591=CARTESIAN_POINT('Ctrl Pts',(0.0381127912063918,0.179863473198069,
0.655768060024794));
#9592=CARTESIAN_POINT('Ctrl Pts',(-0.118305335710584,0.133183342609015,
0.666081736790332));
#9593=CARTESIAN_POINT('Ctrl Pts',(-0.155201794262491,0.0403740370228492,
0.672690509261943));
#9594=CARTESIAN_POINT('Ctrl Pts',(-0.155576082774588,-0.000140575406353826,
0.675594377439629));
#9595=CARTESIAN_POINT('Ctrl Pts',(-0.155599079595997,-0.000137936170561192,
0.61940562256037));
#9596=CARTESIAN_POINT('Ctrl Pts',(-0.155694978954011,-0.0105529059502578,
0.620152394678851));
#9597=CARTESIAN_POINT('Ctrl Pts',(-0.149993983311601,-0.0725344660767061,
0.624604071091256));
#9598=CARTESIAN_POINT('Ctrl Pts',(-0.0668371390874247,-0.171278287625556,
0.632760651797588));
#9599=CARTESIAN_POINT('Ctrl Pts',(0.107664149845629,-0.14903652509151,0.643875364679364));
#9600=CARTESIAN_POINT('Ctrl Pts',(0.183604219596519,0.00964082567459112,
0.654990077561139));
#9601=CARTESIAN_POINT('Ctrl Pts',(0.0914636816765205,0.159492476021631,
0.666104790442917));
#9602=CARTESIAN_POINT('Ctrl Pts',(-0.084407345824762,0.163336630748138,
0.677219503324691));
#9603=CARTESIAN_POINT('Ctrl Pts',(-0.153309057596064,0.0615339443022911,
0.684986447363844));
#9604=CARTESIAN_POINT('Ctrl Pts',(-0.155778971618438,0.00505417110609329,
0.68904848710907));
#9605=CARTESIAN_POINT('Ctrl Pts',(-0.155746091141148,8.5545867844157E-5,
0.689405622560371));
#9606=CARTESIAN_POINT('Origin',(0.,0.,-0.129405622560373));
#9607=CARTESIAN_POINT('',(-0.155620384233268,0.000134389116543367,0.535594377439629));
#9608=CARTESIAN_POINT('',(-0.155294662735063,-4.07947690456786E-7,0.549405622560371));
#9609=CARTESIAN_POINT('',(-0.15555,4.36677073508985E-14,-0.129405622560373));
#9610=CARTESIAN_POINT('Ctrl Pts',(-0.155620384233268,0.000134389116543364,
0.535594377439629));
#9611=CARTESIAN_POINT('Ctrl Pts',(-0.155238150029612,-0.0418142075950562,
0.538603228695431));
#9612=CARTESIAN_POINT('Ctrl Pts',(-0.11609848048108,-0.136044184148923,
0.545316984245157));
#9613=CARTESIAN_POINT('Ctrl Pts',(0.0431815857942205,-0.178714309703255,
0.555735644088809));
#9614=CARTESIAN_POINT('Ctrl Pts',(0.173572271754774,-0.0606310178233981,
0.566850356970585));
#9615=CARTESIAN_POINT('Ctrl Pts',(0.145066103517367,0.112956980548805,0.577965069852361));
#9616=CARTESIAN_POINT('Ctrl Pts',(-0.0162409278223676,0.183138434272774,
0.589079782734138));
#9617=CARTESIAN_POINT('Ctrl Pts',(-0.137582057103126,0.102371477526338,
0.598289551929893));
#9618=CARTESIAN_POINT('Ctrl Pts',(-0.155312980823089,0.0252398494879608,
0.603794416831724));
#9619=CARTESIAN_POINT('Ctrl Pts',(-0.155295522970368,1.20667024935545E-5,
0.605594377439629));
#9620=CARTESIAN_POINT('Ctrl Pts',(-0.155294677199358,-4.07924581107E-7,
0.549405622560371));
#9621=CARTESIAN_POINT('Ctrl Pts',(-0.155295283821613,-0.025939410100839,
0.551256302248632));
#9622=CARTESIAN_POINT('Ctrl Pts',(-0.136845372042004,-0.103805290649511,
0.556811886230819));
#9623=CARTESIAN_POINT('Ctrl Pts',(-0.0137382592728754,-0.183343162418143,
0.56607237450693));
#9624=CARTESIAN_POINT('Ctrl Pts',(0.146595250104258,-0.110965254112288,
0.577187087388706));
#9625=CARTESIAN_POINT('Ctrl Pts',(0.172728038096355,0.0629958715212238,
0.588301800270483));
#9626=CARTESIAN_POINT('Ctrl Pts',(0.0407368261671239,0.179287383736737,
0.599416513152259));
#9627=CARTESIAN_POINT('Ctrl Pts',(-0.117173152128599,0.134664213612,0.609784453915555));
#9628=CARTESIAN_POINT('Ctrl Pts',(-0.155219200688461,0.0411180995720497,
0.616447490384925));
#9629=CARTESIAN_POINT('Ctrl Pts',(-0.155599079595997,-0.000137936170561192,
0.61940562256037));
#9630=CARTESIAN_POINT('Origin',(0.,0.,-0.129405622560373));
#9631=CARTESIAN_POINT('',(-0.155730199251335,-9.53986324873634E-5,0.465594377439629));
#9632=CARTESIAN_POINT('',(-0.155597581791774,0.000138145146615302,0.47940562256037));
#9633=CARTESIAN_POINT('',(-0.15555,4.36677073508985E-14,-0.129405622560373));
#9634=CARTESIAN_POINT('Ctrl Pts',(-0.155730199251335,-9.53986324873637E-5,
0.465594377439629));
#9635=CARTESIAN_POINT('Ctrl Pts',(-0.155771125211943,-0.00577117291295923,
0.466002231971286));
#9636=CARTESIAN_POINT('Ctrl Pts',(-0.15291335048013,-0.0629633964300589,
0.470114990796868));
#9637=CARTESIAN_POINT('Ctrl Pts',(-0.0821687549726806,-0.164474160738562,
0.477932653916376));
#9638=CARTESIAN_POINT('Ctrl Pts',(0.093633366925239,-0.158228462808239,
0.489047366798152));
#9639=CARTESIAN_POINT('Ctrl Pts',(0.183718759405662,-0.00713241101304534,
0.500162079679928));
#9640=CARTESIAN_POINT('Ctrl Pts',(0.105618688669037,0.150493011293707,0.511276792561704));
#9641=CARTESIAN_POINT('Ctrl Pts',(-0.0691700824248357,0.170349504084268,
0.52239150544348));
#9642=CARTESIAN_POINT('Ctrl Pts',(-0.150461957560835,0.0711002170416349,
0.530497367069456));
#9643=CARTESIAN_POINT('Ctrl Pts',(-0.15570880843776,0.00983857377168744,
0.534898324401505));
#9644=CARTESIAN_POINT('Ctrl Pts',(-0.155620384233268,0.000134389116543364,
0.535594377439629));
#9645=CARTESIAN_POINT('Ctrl Pts',(-0.155597581791774,0.000138145146615299,
0.47940562256037));
#9646=CARTESIAN_POINT('Ctrl Pts',(-0.155217974184216,-0.0410694712136483,
0.482360209818413));
#9647=CARTESIAN_POINT('Ctrl Pts',(-0.117247668926727,-0.134567610636498,
0.489019701370381));
#9648=CARTESIAN_POINT('Ctrl Pts',(0.0405656647148524,-0.179326188326124,
0.499384097216273));
#9649=CARTESIAN_POINT('Ctrl Pts',(0.172667825243738,-0.0631607243382489,
0.51049881009805));
#9650=CARTESIAN_POINT('Ctrl Pts',(0.146701107748166,0.110825267691061,0.521613522979825));
#9651=CARTESIAN_POINT('Ctrl Pts',(-0.0135632385845353,0.183356193057212,
0.532728235861603));
#9652=CARTESIAN_POINT('Ctrl Pts',(-0.136793374447236,0.103905470129892,
0.541992269055116));
#9653=CARTESIAN_POINT('Ctrl Pts',(-0.155294069415139,0.0259882795758376,
0.547551397954706));
#9654=CARTESIAN_POINT('Ctrl Pts',(-0.155294677199358,-4.07924581107E-7,
0.549405622560371));
#9655=CARTESIAN_POINT('Origin',(0.,0.,-0.129405622560373));
#9656=CARTESIAN_POINT('',(-0.155329799149561,-7.46101974259461E-5,0.395594377439629));
#9657=CARTESIAN_POINT('',(-0.155747148273957,-8.48283479504552E-5,0.40940562256037));
#9658=CARTESIAN_POINT('',(-0.15555,4.36677073508985E-14,-0.129405622560373));
#9659=CARTESIAN_POINT('Ctrl Pts',(-0.155329799149561,-7.46101974259585E-5,
0.395594377439629));
#9660=CARTESIAN_POINT('Ctrl Pts',(-0.155421611019211,-0.0212513995734132,
0.397106139541067));
#9661=CARTESIAN_POINT('Ctrl Pts',(-0.141514901582445,-0.0942110799989907,
0.40232280593643));
#9662=CARTESIAN_POINT('Ctrl Pts',(-0.030390408656302,-0.18132809188354,
0.411244376625719));
#9663=CARTESIAN_POINT('Ctrl Pts',(0.135872146613563,-0.123863689671489,
0.422359089507495));
#9664=CARTESIAN_POINT('Ctrl Pts',(0.177750452880091,0.0469918114711103,
0.433473802389271));
#9665=CARTESIAN_POINT('Ctrl Pts',(0.0569069861965436,0.174828626850531,
0.444588515271047));
#9666=CARTESIAN_POINT('Ctrl Pts',(-0.109686020656632,0.143800409504297,
0.455295373621167));
#9667=CARTESIAN_POINT('Ctrl Pts',(-0.15539935842889,0.045786916726629,0.46229732767736));
#9668=CARTESIAN_POINT('Ctrl Pts',(-0.155730199251335,-9.53986324873637E-5,
0.465594377439629));
#9669=CARTESIAN_POINT('Ctrl Pts',(-0.155747148273957,-8.48283479504535E-5,
0.40940562256037));
#9670=CARTESIAN_POINT('Ctrl Pts',(-0.155779482799656,-0.00500404714443213,
0.409759213094268));
#9671=CARTESIAN_POINT('Ctrl Pts',(-0.153336323268121,-0.0614340654297066,
0.413817707922091));
#9672=CARTESIAN_POINT('Ctrl Pts',(-0.0845632241029054,-0.163255983359439,
0.42158110704384));
#9673=CARTESIAN_POINT('Ctrl Pts',(0.0913113927969153,-0.159579712115361,
0.432695819925616));
#9674=CARTESIAN_POINT('Ctrl Pts',(0.183594933073833,-0.00981608490943425,
0.443810532807392));
#9675=CARTESIAN_POINT('Ctrl Pts',(0.107806367033371,0.148933683901261,0.454925245689169));
#9676=CARTESIAN_POINT('Ctrl Pts',(-0.0666736110104746,0.171342010517439,
0.466039958570945));
#9677=CARTESIAN_POINT('Ctrl Pts',(-0.149960857132942,0.0726347328707636,
0.474200084194679));
#9678=CARTESIAN_POINT('Ctrl Pts',(-0.155693983092541,0.0106028137662625,
0.478655305524487));
#9679=CARTESIAN_POINT('Ctrl Pts',(-0.155597581791774,0.000138145146615299,
0.47940562256037));
#9680=CARTESIAN_POINT('Origin',(0.,0.,-0.129405622560373));
#9681=CARTESIAN_POINT('',(-0.155457619458094,0.000134802415058048,0.325594377439629));
#9682=CARTESIAN_POINT('',(-0.155341574103549,-8.50015047459685E-5,0.33940562256037));
#9683=CARTESIAN_POINT('',(-0.15555,4.36677073508985E-14,-0.129405622560373));
#9684=CARTESIAN_POINT('Ctrl Pts',(-0.155457619458094,0.000134802415058059,
0.325594377439629));
#9685=CARTESIAN_POINT('Ctrl Pts',(-0.155154675739571,-0.0364297795001245,
0.328210047110848));
#9686=CARTESIAN_POINT('Ctrl Pts',(-0.124018139179925,-0.125249838662379,
0.334530621075992));
#9687=CARTESIAN_POINT('Ctrl Pts',(0.0240536163419306,-0.182276924995041,
0.344556099335061));
#9688=CARTESIAN_POINT('Ctrl Pts',(0.166192972555312,-0.078634278260764,
0.355670812216838));
#9689=CARTESIAN_POINT('Ctrl Pts',(0.156190859040095,0.0969941719726652,
0.366785525098613));
#9690=CARTESIAN_POINT('Ctrl Pts',(0.00320371741518769,0.183829241523736,
0.37790023798039));
#9691=CARTESIAN_POINT('Ctrl Pts',(-0.131508890630062,0.113456296578242,
0.387503188760728));
#9692=CARTESIAN_POINT('Ctrl Pts',(-0.15519660591439,0.0306469631491546,
0.393401235247141));
#9693=CARTESIAN_POINT('Ctrl Pts',(-0.155329799149561,-7.46101974259585E-5,
0.395594377439629));
#9694=CARTESIAN_POINT('Ctrl Pts',(-0.155341574103549,-8.50015047459546E-5,
0.33940562256037));
#9695=CARTESIAN_POINT('Ctrl Pts',(-0.15544287226748,-0.0204977876623303,
0.340863120664049));
#9696=CARTESIAN_POINT('Ctrl Pts',(-0.142208294129094,-0.0926729514204939,
0.346025523061653));
#9697=CARTESIAN_POINT('Ctrl Pts',(-0.0330366684018241,-0.180864682882801,
0.354892829753183));
#9698=CARTESIAN_POINT('Ctrl Pts',(0.134047790173482,-0.125835785541829,
0.366007542634959));
#9699=CARTESIAN_POINT('Ctrl Pts',(0.178418108088907,0.0443895672348972,
0.377122255516735));
#9700=CARTESIAN_POINT('Ctrl Pts',(0.0594554476394192,0.173978460503991,
0.388236968398511));
#9701=CARTESIAN_POINT('Ctrl Pts',(-0.108419677339067,0.145242852620103,
0.39899809074639));
#9702=CARTESIAN_POINT('Ctrl Pts',(-0.155440683223253,0.0465392864424033,
0.406054308800343));
#9703=CARTESIAN_POINT('Ctrl Pts',(-0.155747148273957,-8.48283479504535E-5,
0.40940562256037));
#9704=CARTESIAN_POINT('Origin',(0.,0.,-0.129405622560373));
#9705=CARTESIAN_POINT('',(-0.15580501159203,-3.81191605503711E-6,0.255594377439629));
#9706=CARTESIAN_POINT('',(-0.155437230887358,0.000130168175253818,0.26940562256037));
#9707=CARTESIAN_POINT('',(-0.15555,4.36677073508985E-14,-0.129405622560373));
#9708=CARTESIAN_POINT('Ctrl Pts',(-0.15580501159203,-3.81191605504483E-6,
0.255594377439629));
#9709=CARTESIAN_POINT('Ctrl Pts',(-0.155805085024067,-0.000207743207977253,
0.255609050386703));
#9710=CARTESIAN_POINT('Ctrl Pts',(-0.15571236399541,-0.05190405066865,0.259328627627703));
#9711=CARTESIAN_POINT('Ctrl Pts',(-0.0990899426121504,-0.154869742320406,
0.266753109162628));
#9712=CARTESIAN_POINT('Ctrl Pts',(0.0763877910491314,-0.167237433721381,
0.277867822044404));
#9713=CARTESIAN_POINT('Ctrl Pts',(0.181936269483671,-0.0265075025422269,
0.288982534926181));
#9714=CARTESIAN_POINT('Ctrl Pts',(0.120931066297065,0.138488739775033,0.300097247807957));
#9715=CARTESIAN_POINT('Ctrl Pts',(-0.0507805637499992,0.17670537114635,
0.311211960689733));
#9716=CARTESIAN_POINT('Ctrl Pts',(-0.146535504929177,0.0822320925013407,
0.31971100390029));
#9717=CARTESIAN_POINT('Ctrl Pts',(-0.155583773303352,0.0153612696655085,
0.324505142816922));
#9718=CARTESIAN_POINT('Ctrl Pts',(-0.155457619458094,0.000134802415058059,
0.325594377439629));
#9719=CARTESIAN_POINT('Ctrl Pts',(-0.155437230887358,0.00013016817525382,
0.26940562256037));
#9720=CARTESIAN_POINT('Ctrl Pts',(-0.155153480292112,-0.0356877371401405,
0.27196702823383));
#9721=CARTESIAN_POINT('Ctrl Pts',(-0.125038150141719,-0.1237447022416,0.278233338201215));
#9722=CARTESIAN_POINT('Ctrl Pts',(0.0213876812582842,-0.182608932054395,
0.288204552462526));
#9723=CARTESIAN_POINT('Ctrl Pts',(0.1650262562684,-0.0810542393413567,0.299319265344302));
#9724=CARTESIAN_POINT('Ctrl Pts',(0.157591432764151,0.0947016118771478,
0.310433978226078));
#9725=CARTESIAN_POINT('Ctrl Pts',(0.00588942498427058,0.183762808117002,
0.321548691107855));
#9726=CARTESIAN_POINT('Ctrl Pts',(-0.130604027396502,0.114979253369884,
0.331205905885952));
#9727=CARTESIAN_POINT('Ctrl Pts',(-0.155185376218898,0.031390732051916,
0.337158216370124));
#9728=CARTESIAN_POINT('Ctrl Pts',(-0.155341574103549,-8.50015047459546E-5,
0.33940562256037));
#9729=CARTESIAN_POINT('Origin',(0.,0.,-0.129405622560373));
#9730=CARTESIAN_POINT('',(-0.155446481294809,-0.000132426206499563,0.185594377439629));
#9731=CARTESIAN_POINT('',(-0.155804282564045,1.0275387755743E-5,0.19940562256037));
#9732=CARTESIAN_POINT('',(-0.15555,4.36677073508985E-14,-0.129405622560373));
#9733=CARTESIAN_POINT('Ctrl Pts',(-0.155446481294809,-0.000132426206499552,
0.185594377439629));
#9734=CARTESIAN_POINT('Ctrl Pts',(-0.15557308597482,-0.0157719577277014,
0.186712957956484));
#9735=CARTESIAN_POINT('Ctrl Pts',(-0.14621431385393,-0.0830638986146384,
0.191536442767265));
#9736=CARTESIAN_POINT('Ctrl Pts',(-0.0493826231024586,-0.177101125876806,
0.200064831871971));
#9737=CARTESIAN_POINT('Ctrl Pts',(0.122021650540482,-0.137528801235027,
0.211179544753747));
#9738=CARTESIAN_POINT('Ctrl Pts',(0.181721122596515,0.027944365932959,0.222294257635524));
#9739=CARTESIAN_POINT('Ctrl Pts',(0.0750638686912215,0.167835840141849,
0.2334089705173));
#9740=CARTESIAN_POINT('Ctrl Pts',(-0.10007913601891,0.154100039675233,0.244509010452001));
#9741=CARTESIAN_POINT('Ctrl Pts',(-0.155786543508857,0.0512847017165995,
0.251904146092778));
#9742=CARTESIAN_POINT('Ctrl Pts',(-0.15580501159203,-3.81191605504483E-6,
0.255594377439629));
#9743=CARTESIAN_POINT('Ctrl Pts',(-0.155804282564045,1.02753877557394E-5,
0.19940562256037));
#9744=CARTESIAN_POINT('Ctrl Pts',(-0.155755696547123,-0.0509325620518932,
0.203070935803611));
#9745=CARTESIAN_POINT('Ctrl Pts',(-0.100717920681623,-0.153458525692979,
0.210441153340777));
#9746=CARTESIAN_POINT('Ctrl Pts',(0.0739360216217259,-0.168335735272026,
0.221516275171869));
#9747=CARTESIAN_POINT('Ctrl Pts',(0.181529531305135,-0.0291630630877277,
0.232630988053645));
#9748=CARTESIAN_POINT('Ctrl Pts',(0.122941707923409,0.13670695445041,0.243745700935421));
#9749=CARTESIAN_POINT('Ctrl Pts',(-0.0481931854649256,0.177428497887793,
0.254860413817197));
#9750=CARTESIAN_POINT('Ctrl Pts',(-0.145938433460327,0.0837702536114789,
0.263413721025514));
#9751=CARTESIAN_POINT('Ctrl Pts',(-0.155563906805031,0.0161204994767368,
0.268262123939905));
#9752=CARTESIAN_POINT('Ctrl Pts',(-0.155437230887358,0.00013016817525382,
0.26940562256037));
#9753=CARTESIAN_POINT('Origin',(0.,0.,-0.129405622560373));
#9754=CARTESIAN_POINT('',(-0.15533593717049,8.0492722526641E-5,0.115594377439629));
#9755=CARTESIAN_POINT('',(-0.155467267562279,-0.000136569073934972,0.12940562256037));
#9756=CARTESIAN_POINT('',(-0.15555,4.36677073508985E-14,-0.129405622560373));
#9757=CARTESIAN_POINT('Ctrl Pts',(-0.15533593717049,8.04927225266511E-5,
0.115594377439629));
#9758=CARTESIAN_POINT('Ctrl Pts',(-0.155190332415358,-0.0310491436783933,
0.117816865526265));
#9759=CARTESIAN_POINT('Ctrl Pts',(-0.131021645937763,-0.114280472202705,
0.123744257906827));
#9760=CARTESIAN_POINT('Ctrl Pts',(0.00465630089802304,-0.183797982260963,
0.133376554581314));
#9761=CARTESIAN_POINT('Ctrl Pts',(0.156952427521129,-0.0957570050449602,
0.14449126746309));
#9762=CARTESIAN_POINT('Ctrl Pts',(0.165566412512777,0.0799451630251659,
0.155605980344867));
#9763=CARTESIAN_POINT('Ctrl Pts',(0.0226124784964766,0.182461279865869,
0.166720693226643));
#9764=CARTESIAN_POINT('Ctrl Pts',(-0.124571916682485,0.124436273223993,
0.176716825591564));
#9765=CARTESIAN_POINT('Ctrl Pts',(-0.155153752528961,0.036028486330431,
0.183008053662559));
#9766=CARTESIAN_POINT('Ctrl Pts',(-0.155446481294809,-0.000132426206499552,
0.185594377439629));
#9767=CARTESIAN_POINT('Ctrl Pts',(-0.155467267562279,-0.000136569073934965,
0.12940562256037));
#9768=CARTESIAN_POINT('Ctrl Pts',(-0.155592737404977,-0.0150123740177689,
0.130469939079467));
#9769=CARTESIAN_POINT('Ctrl Pts',(-0.146805111767969,-0.0815259022509084,
0.135239159892488));
#9770=CARTESIAN_POINT('Ctrl Pts',(-0.0519650836355626,-0.176360636356525,
0.143713284999436));
#9771=CARTESIAN_POINT('Ctrl Pts',(0.119999097845339,-0.139297072446483,
0.154827997881212));
#9772=CARTESIAN_POINT('Ctrl Pts',(0.182110041762725,0.0252861433827556,
0.165942710762988));
#9773=CARTESIAN_POINT('Ctrl Pts',(0.0775082145815245,0.166721114602665,
0.177057423644764));
#9774=CARTESIAN_POINT('Ctrl Pts',(-0.0980485553243366,0.155531142530291,
0.18817213652654));
#9775=CARTESIAN_POINT('Ctrl Pts',(-0.15555294238022,0.0526034030257051,
0.195621536165076));
#9776=CARTESIAN_POINT('Ctrl Pts',(-0.155804807368156,0.000560536804787789,
0.199366031509686));
#9777=CARTESIAN_POINT('Ctrl Pts',(-0.155804282564045,1.02753877557394E-5,
0.19940562256037));
#9778=CARTESIAN_POINT('Origin',(0.,0.,-0.129405622560373));
#9779=CARTESIAN_POINT('',(-0.155737693224454,0.000100603112028587,0.045594377439629));
#9780=CARTESIAN_POINT('',(-0.155324515707295,7.08434145518383E-5,0.0594056225603703));
#9781=CARTESIAN_POINT('',(-0.15555,4.36677073508985E-14,-0.129405622560373));
#9782=CARTESIAN_POINT('Ctrl Pts',(-0.155737693224454,0.000100603112028588,
0.045594377439629));
#9783=CARTESIAN_POINT('Ctrl Pts',(-0.155418890749049,-0.0461799127824949,
0.0489207730960463));
#9784=CARTESIAN_POINT('Ctrl Pts',(-0.109006528319361,-0.14459862692607,
0.055952073046389));
#9785=CARTESIAN_POINT('Ctrl Pts',(0.0582883981674798,-0.17436384297299,
0.0666882772906571));
#9786=CARTESIAN_POINT('Ctrl Pts',(0.178115364857574,-0.0455907972452466,
0.0778029901724332));
#9787=CARTESIAN_POINT('Ctrl Pts',(0.134889573452136,0.124936168947966,0.0889177030542095));
#9788=CARTESIAN_POINT('Ctrl Pts',(-0.0318225855039178,0.181080880580275,
0.100032415935985));
#9789=CARTESIAN_POINT('Ctrl Pts',(-0.141891652849943,0.0933796088184345,
0.108924640731125));
#9790=CARTESIAN_POINT('Ctrl Pts',(-0.155433056633206,0.0208441934619002,
0.11411196123234));
#9791=CARTESIAN_POINT('Ctrl Pts',(-0.15533593717049,8.04927225266511E-5,
0.115594377439629));
#9792=CARTESIAN_POINT('Ctrl Pts',(-0.155324515707295,7.08434145518418E-5,
0.0594056225603703));
#9793=CARTESIAN_POINT('Ctrl Pts',(-0.155202011031474,-0.0303045958272501,
0.0615738466492476));
#9794=CARTESIAN_POINT('Ctrl Pts',(-0.131919585929676,-0.112758296333805,
0.0674469750320503));
#9795=CARTESIAN_POINT('Ctrl Pts',(0.00197063906297734,-0.183845261801054,
0.0770250077087785));
#9796=CARTESIAN_POINT('Ctrl Pts',(0.155536281225319,-0.0980407171232175,
0.0881397205905545));
#9797=CARTESIAN_POINT('Ctrl Pts',(0.166716989499632,0.0775177448756012,
0.0992544334723309));
#9798=CARTESIAN_POINT('Ctrl Pts',(0.0252760640494928,0.182111233028749,
0.110369146354107));
#9799=CARTESIAN_POINT('Ctrl Pts',(-0.12354388404776,0.125939975141946,0.120419542716787));
#9800=CARTESIAN_POINT('Ctrl Pts',(-0.15515597470269,0.0367705614371862,
0.126765034785541));
#9801=CARTESIAN_POINT('Ctrl Pts',(-0.155467267562279,-0.000136569073934965,
0.12940562256037));
#9802=CARTESIAN_POINT('Ctrl Pts',(-0.0685825729128552,0.139614588036684,
-0.0230074082272072));
#9803=CARTESIAN_POINT('Ctrl Pts',(-0.115011604060829,0.116807355219849,
-0.0193025039332818));
#9804=CARTESIAN_POINT('Ctrl Pts',(-0.18252632432761,0.0216311623708125,
-0.011892695345431));
#9805=CARTESIAN_POINT('Ctrl Pts',(-0.117028832316993,-0.141960369302502,
-0.00077798246365487));
#9806=CARTESIAN_POINT('Ctrl Pts',(0.0557547713450657,-0.175142639980632,
0.0103367304181214));
#9807=CARTESIAN_POINT('Ctrl Pts',(0.177419525591119,-0.0482168938798953,
0.0214514432998975));
#9808=CARTESIAN_POINT('Ctrl Pts',(0.13670630608002,0.122966787890628,0.0325661561816737));
#9809=CARTESIAN_POINT('Ctrl Pts',(-0.0291762440449378,0.181518694867924,
0.0436808690634499));
#9810=CARTESIAN_POINT('Ctrl Pts',(-0.168338109470647,0.0739316281669151,
0.0547955819452261));
#9811=CARTESIAN_POINT('Ctrl Pts',(-0.153400663029731,-0.101353247263981,
0.0659102948270022));
#9812=CARTESIAN_POINT('Ctrl Pts',(0.00197063906297734,-0.183845261801054,
0.0770250077087785));
#9813=CARTESIAN_POINT('Ctrl Pts',(0.155536281225319,-0.0980407171232175,
0.0881397205905545));
#9814=CARTESIAN_POINT('Ctrl Pts',(0.166716989499632,0.0775177448756012,
0.0992544334723309));
#9815=CARTESIAN_POINT('Ctrl Pts',(0.0252760640494928,0.182111233028749,
0.110369146354107));
#9816=CARTESIAN_POINT('Ctrl Pts',(-0.13930361365595,0.119991553257876,0.121483859235883));
#9817=CARTESIAN_POINT('Ctrl Pts',(-0.176357828501591,-0.0519748351675156,
0.132598572117659));
#9818=CARTESIAN_POINT('Ctrl Pts',(-0.0519650836355626,-0.176360636356525,
0.143713284999436));
#9819=CARTESIAN_POINT('Ctrl Pts',(0.119999097845339,-0.139297072446483,
0.154827997881212));
#9820=CARTESIAN_POINT('Ctrl Pts',(0.182110041762725,0.0252861433827556,
0.165942710762988));
#9821=CARTESIAN_POINT('Ctrl Pts',(0.0775082145815245,0.166721114602665,
0.177057423644764));
#9822=CARTESIAN_POINT('Ctrl Pts',(-0.0980485553243366,0.155531142530291,
0.18817213652654));
#9823=CARTESIAN_POINT('Ctrl Pts',(-0.183846711227048,0.00196007268919948,
0.199286849408317));
#9824=CARTESIAN_POINT('Ctrl Pts',(-0.101342268945007,-0.15340534304023,
0.210401562290092));
#9825=CARTESIAN_POINT('Ctrl Pts',(0.0739360216217259,-0.168335735272026,
0.221516275171869));
#9826=CARTESIAN_POINT('Ctrl Pts',(0.181529531305135,-0.0291630630877277,
0.232630988053645));
#9827=CARTESIAN_POINT('Ctrl Pts',(0.122941707923409,0.13670695445041,0.243745700935421));
#9828=CARTESIAN_POINT('Ctrl Pts',(-0.0481931854649256,0.177428497887793,
0.254860413817197));
#9829=CARTESIAN_POINT('Ctrl Pts',(-0.175209594506165,0.055723002131679,
0.265975126698974));
#9830=CARTESIAN_POINT('Ctrl Pts',(-0.141830261094154,-0.116994153730485,
0.27708983958075));
#9831=CARTESIAN_POINT('Ctrl Pts',(0.0213876812582842,-0.182608932054395,
0.288204552462526));
#9832=CARTESIAN_POINT('Ctrl Pts',(0.1650262562684,-0.0810542393413567,0.299319265344302));
#9833=CARTESIAN_POINT('Ctrl Pts',(0.157591432764151,0.0947016118771478,
0.310433978226078));
#9834=CARTESIAN_POINT('Ctrl Pts',(0.00588942498427058,0.183762808117002,
0.321548691107855));
#9835=CARTESIAN_POINT('Ctrl Pts',(-0.151204060903134,0.104598216713686,
0.332663403989631));
#9836=CARTESIAN_POINT('Ctrl Pts',(-0.169877686425305,-0.0703208832997102,
0.343778116871407));
#9837=CARTESIAN_POINT('Ctrl Pts',(-0.0330366684018241,-0.180864682882801,
0.354892829753183));
#9838=CARTESIAN_POINT('Ctrl Pts',(0.134047790173482,-0.125835785541829,
0.366007542634959));
#9839=CARTESIAN_POINT('Ctrl Pts',(0.178418108088907,0.0443895672348972,
0.377122255516735));
#9840=CARTESIAN_POINT('Ctrl Pts',(0.0594554476394192,0.173978460503991,
0.388236968398511));
#9841=CARTESIAN_POINT('Ctrl Pts',(-0.11393574277819,0.144298653808392,0.399351681280288));
#9842=CARTESIAN_POINT('Ctrl Pts',(-0.183024379999154,-0.0174794536315888,
0.410466394162064));
#9843=CARTESIAN_POINT('Ctrl Pts',(-0.0845632241029054,-0.163255983359439,
0.42158110704384));
#9844=CARTESIAN_POINT('Ctrl Pts',(0.0913113927969153,-0.159579712115361,
0.432695819925616));
#9845=CARTESIAN_POINT('Ctrl Pts',(0.183594933073833,-0.00981608490943425,
0.443810532807392));
#9846=CARTESIAN_POINT('Ctrl Pts',(0.107806367033371,0.148933683901261,0.454925245689169));
#9847=CARTESIAN_POINT('Ctrl Pts',(-0.0666736110104746,0.171342010517439,
0.466039958570945));
#9848=CARTESIAN_POINT('Ctrl Pts',(-0.180117186520217,0.0368951771018348,
0.477154671452721));
#9849=CARTESIAN_POINT('Ctrl Pts',(-0.128672361159773,-0.131327371278433,
0.488269384334498));
#9850=CARTESIAN_POINT('Ctrl Pts',(0.0405656647148524,-0.179326188326124,
0.499384097216273));
#9851=CARTESIAN_POINT('Ctrl Pts',(0.172667825243738,-0.0631607243382489,
0.51049881009805));
#9852=CARTESIAN_POINT('Ctrl Pts',(0.146701107748166,0.110825267691061,0.521613522979825));
#9853=CARTESIAN_POINT('Ctrl Pts',(-0.0135632385845353,0.183356193057212,
0.532728235861603));
#9854=CARTESIAN_POINT('Ctrl Pts',(-0.161411108932732,0.0880335668165284,
0.543842948743377));
#9855=CARTESIAN_POINT('Ctrl Pts',(-0.161495069857358,-0.0878794480245611,
0.554957661625155));
#9856=CARTESIAN_POINT('Ctrl Pts',(-0.0137382592728754,-0.183343162418143,
0.56607237450693));
#9857=CARTESIAN_POINT('Ctrl Pts',(0.146595250104258,-0.110965254112288,
0.577187087388706));
#9858=CARTESIAN_POINT('Ctrl Pts',(0.172728038096355,0.0629958715212238,
0.588301800270483));
#9859=CARTESIAN_POINT('Ctrl Pts',(0.0407368261671239,0.179287383736737,
0.599416513152259));
#9860=CARTESIAN_POINT('Ctrl Pts',(-0.12854694097571,0.131450138604423,0.610531226034035));
#9861=CARTESIAN_POINT('Ctrl Pts',(-0.180152323597142,-0.0367232252925209,
0.621645938915811));
#9862=CARTESIAN_POINT('Ctrl Pts',(-0.0668371390874247,-0.171278287625556,
0.632760651797588));
#9863=CARTESIAN_POINT('Ctrl Pts',(0.107664149845629,-0.14903652509151,0.643875364679364));
#9864=CARTESIAN_POINT('Ctrl Pts',(0.183604219596519,0.00964082567459112,
0.654990077561139));
#9865=CARTESIAN_POINT('Ctrl Pts',(0.0914636816765205,0.159492476021631,
0.666104790442917));
#9866=CARTESIAN_POINT('Ctrl Pts',(-0.084407345824762,0.163336630748138,
0.677219503324691));
#9867=CARTESIAN_POINT('Ctrl Pts',(-0.183007611198191,0.0176541557959064,
0.688334216206469));
#9868=CARTESIAN_POINT('Ctrl Pts',(-0.114073434464645,-0.144189828083589,
0.699448929088244));
#9869=CARTESIAN_POINT('Ctrl Pts',(0.0592893454135225,-0.174035135802431,
0.710563641970021));
#9870=CARTESIAN_POINT('Ctrl Pts',(0.17837565371923,-0.0445598601161589,
0.721678354851797));
#9871=CARTESIAN_POINT('Ctrl Pts',(0.134167848541566,0.125707769811822,0.732793067733573));
#9872=CARTESIAN_POINT('Ctrl Pts',(-0.0328640048105861,0.18089613639087,
0.743907780615349));
#9873=CARTESIAN_POINT('Ctrl Pts',(-0.169810482613085,0.0704830119109969,
0.755022493497126));
#9874=CARTESIAN_POINT('Ctrl Pts',(-0.151303838645199,-0.104453833747555,
0.766137206378901));
#9875=CARTESIAN_POINT('Ctrl Pts',(0.0057140072891202,-0.183768346278771,
0.777251919260679));
#9876=CARTESIAN_POINT('Ctrl Pts',(0.157500961365389,-0.0948520012562343,
0.788366632142453));
#9877=CARTESIAN_POINT('Ctrl Pts',(0.165103553267307,0.080896672810716,0.799481345024232));
#9878=CARTESIAN_POINT('Ctrl Pts',(0.0215619850688987,0.182588432747595,
0.810596057906006));
#9879=CARTESIAN_POINT('Ctrl Pts',(-0.141718517021854,0.117129487775116,
0.821710770787783));
#9880=CARTESIAN_POINT('Ctrl Pts',(-0.17526270634378,-0.0555557264230108,
0.832825483669558));
#9881=CARTESIAN_POINT('Ctrl Pts',(-0.0483625319738309,-0.177382413092208,
0.843940196551336));
#9882=CARTESIAN_POINT('Ctrl Pts',(0.122811155175551,-0.136824249085392,
0.855054909433111));
#9883=CARTESIAN_POINT('Ctrl Pts',(0.18155728681432,0.0289897667799704,0.866169622314888));
#9884=CARTESIAN_POINT('Ctrl Pts',(0.0740966767894734,0.168265080935085,
0.877284335196663));
#9885=CARTESIAN_POINT('Ctrl Pts',(-0.101195786384157,0.153502012336733,
0.88839904807844));
#9886=CARTESIAN_POINT('Ctrl Pts',(-0.183848498104576,-0.00178457782861093,
0.899513760960216));
#9887=CARTESIAN_POINT('Ctrl Pts',(-0.0981969772278097,-0.155437475007334,
0.910628473841992));
#9888=CARTESIAN_POINT('Ctrl Pts',(0.0773490332209564,-0.16679503000125,
0.921743186723768));
#9889=CARTESIAN_POINT('Ctrl Pts',(0.182085818614306,-0.0254599613686364,
0.932857899605545));
#9890=CARTESIAN_POINT('Ctrl Pts',(0.120132017548368,0.139182446210336,0.943972612487321));
#9891=CARTESIAN_POINT('Ctrl Pts',(-0.0517967206657041,0.176410188769281,
0.955087325369096));
#9892=CARTESIAN_POINT('Ctrl Pts',(-0.1763081157273,0.0521431040696983,0.966202038250874));
#9893=CARTESIAN_POINT('Ctrl Pts',(-0.139418126366054,-0.11985842070507,
0.977316751132648));
#9894=CARTESIAN_POINT('Ctrl Pts',(0.0251022815740214,-0.182135472747933,
0.988431464014426));
#9895=CARTESIAN_POINT('Ctrl Pts',(0.166642788778922,-0.0776764824211173,
0.999546176896201));
#9896=CARTESIAN_POINT('Ctrl Pts',(0.155630041687788,0.0978914965540504,
1.01066088977798));
#9897=CARTESIAN_POINT('Ctrl Pts',(0.00214566711329121,0.183844638447722,
1.02177560265976));
#9898=CARTESIAN_POINT('Ctrl Pts',(-0.153302959879009,0.1014970810697,1.03289031554153));
#9899=CARTESIAN_POINT('Ctrl Pts',(-0.168410288012087,-0.073766048186277,
1.04400502842331));
#9900=CARTESIAN_POINT('Ctrl Pts',(-0.0293463034743252,-0.181499998473078,
1.05511974130508));
#9901=CARTESIAN_POINT('Ctrl Pts',(0.136582774532958,-0.123079651747206,
1.06623445418686));
#9902=CARTESIAN_POINT('Ctrl Pts',(0.177477058724911,0.048014045858363,1.07734916706863));
#9903=CARTESIAN_POINT('Ctrl Pts',(0.0558998488320383,0.175153252535857,
1.08846387995041));
#9904=CARTESIAN_POINT('Ctrl Pts',(-0.116850915683094,0.141948295084362,
1.09957859283219));
#9905=CARTESIAN_POINT('Ctrl Pts',(-0.182630429983634,-0.0212033256195195,
1.11069330571396));
#9906=CARTESIAN_POINT('Ctrl Pts',(-0.0812207929765285,-0.164944347467861,
1.12180801859574));
#9907=CARTESIAN_POINT('Ctrl Pts',(0.0945424741868258,-0.15768695427323,
1.13292273147752));
#9908=CARTESIAN_POINT('Ctrl Pts',(0.183756769071919,-0.00607493157030043,
1.14403744435929));
#9909=CARTESIAN_POINT('Ctrl Pts',(0.104750804765144,0.151098391369297,1.15515215724107));
#9910=CARTESIAN_POINT('Ctrl Pts',(-0.0701493549889435,0.169948589190878,
1.16626687012284));
#9911=CARTESIAN_POINT('Ctrl Pts',(-0.180831240020515,0.033219235481529,
1.17738158300462));
#9912=CARTESIAN_POINT('Ctrl Pts',(-0.125971043419533,-0.133920689936726,
1.1884962958864));
#9913=CARTESIAN_POINT('Ctrl Pts',(0.0442094305335735,-0.178462828693349,
1.19961100876817));
#9914=CARTESIAN_POINT('Ctrl Pts',(0.173918351244622,-0.0596310495772682,
1.21072572164995));
#9915=CARTESIAN_POINT('Ctrl Pts',(0.144413599053411,0.113790014420313,1.22184043453173));
#9916=CARTESIAN_POINT('Ctrl Pts',(-0.0172946805849302,0.183041932345569,
1.2329551474135));
#9917=CARTESIAN_POINT('Ctrl Pts',(-0.16317053312232,0.0847279888461446,
1.24406986029528));
#9918=CARTESIAN_POINT('Ctrl Pts',(-0.159671810165464,-0.0911502496530778,
1.25518457317705));
#9919=CARTESIAN_POINT('Ctrl Pts',(-0.0100014200241654,-0.183584930129994,
1.26629928605883));
#9920=CARTESIAN_POINT('Ctrl Pts',(0.148824776878697,-0.107956661491269,
1.2774139989406));
#9921=CARTESIAN_POINT('Ctrl Pts',(0.171409230594902,0.0665006063145147,
1.28852871182238));
#9922=CARTESIAN_POINT('Ctrl Pts',(0.0370769876137034,0.180079848852746,
1.29964342470416));
#9923=CARTESIAN_POINT('Ctrl Pts',(-0.13119740888887,0.128804871313864,1.31075813758594));
#9924=CARTESIAN_POINT('Ctrl Pts',(-0.17936704821676,-0.0403846132498615,
1.32187285046771));
#9925=CARTESIAN_POINT('Ctrl Pts',(-0.0633350012944175,-0.172603976154579,
1.33298756334949));
#9926=CARTESIAN_POINT('Ctrl Pts',(0.110677115627384,-0.146812911726923,
1.34410227623126));
#9927=CARTESIAN_POINT('Ctrl Pts',(0.183369791793454,0.0133781325662369,
1.35521698911304));
#9928=CARTESIAN_POINT('Ctrl Pts',(0.0881964673803512,0.161322156305205,
1.36633170199482));
#9929=CARTESIAN_POINT('Ctrl Pts',(-0.087716373065073,0.161583702363956,
1.37744641487659));
#9930=CARTESIAN_POINT('Ctrl Pts',(-0.183329200145536,0.013923338225167,
1.38856112775837));
#9931=CARTESIAN_POINT('Ctrl Pts',(-0.111113186298513,-0.146483155358991,
1.39967584064014));
#9932=CARTESIAN_POINT('Ctrl Pts',(0.062821469496632,-0.172791544768887,
1.41079055352192));
#9933=CARTESIAN_POINT('Ctrl Pts',(0.179246168325776,-0.0409177970309031,
1.4219052664037));
#9934=CARTESIAN_POINT('Ctrl Pts',(0.131579840483081,0.12841417582098,1.43301997928547));
#9935=CARTESIAN_POINT('Ctrl Pts',(-0.0365413417972516,0.180189304102632,
1.44413469216725));
#9936=CARTESIAN_POINT('Ctrl Pts',(-0.171210727883091,0.0670100114242395,
1.45524940504903));
#9937=CARTESIAN_POINT('Ctrl Pts',(-0.149145136714026,-0.107513641775772,
1.4663641179308));
#9938=CARTESIAN_POINT('Ctrl Pts',(0.00945547127077659,-0.183613858508507,
1.47747883081258));
#9939=CARTESIAN_POINT('Ctrl Pts',(0.159400061651521,-0.0916246436218211,
1.48859354369435));
#9940=CARTESIAN_POINT('Ctrl Pts',(0.163421757209686,0.0842424135684204,
1.49970825657613));
#9941=CARTESIAN_POINT('Ctrl Pts',(0.0178388940120074,0.182989695977022,
1.51082296945791));
#9942=CARTESIAN_POINT('Ctrl Pts',(-0.144074596838477,0.114218936780048,
1.52193768233968));
#9943=CARTESIAN_POINT('Ctrl Pts',(-0.174094900049997,-0.059113625755116,
1.53305239522146));
#9944=CARTESIAN_POINT('Ctrl Pts',(-0.0447399086353324,-0.178330579398589,
1.54416710810323));
#9945=CARTESIAN_POINT('Ctrl Pts',(0.125572262560343,-0.134294682876169,
1.55528182098501));
#9946=CARTESIAN_POINT('Ctrl Pts',(0.180929220612589,0.0326813723985916,
1.56639653386679));
#9947=CARTESIAN_POINT('Ctrl Pts',(0.0706544006326465,0.16973924308944,1.57751124674856));
#9948=CARTESIAN_POINT('Ctrl Pts',(-0.104301038447746,0.151409208280264,
1.58862595963034));
#9949=CARTESIAN_POINT('Ctrl Pts',(-0.183774020961904,-0.0055284891994118,
1.59974067251211));
#9950=CARTESIAN_POINT('Ctrl Pts',(-0.0950109510297781,-0.157405127482403,
1.61085538539389));
#9951=CARTESIAN_POINT('Ctrl Pts',(0.08072995862503,-0.165185134784385,1.62197009827567));
#9952=CARTESIAN_POINT('Ctrl Pts',(0.18256657276441,-0.0217462981307606,
1.63308481115744));
#9953=CARTESIAN_POINT('Ctrl Pts',(0.117272493730902,0.141600201933013,1.64419952403922));
#9954=CARTESIAN_POINT('Ctrl Pts',(-0.0553787694277143,0.175318700856487,
1.65531423692099));
#9955=CARTESIAN_POINT('Ctrl Pts',(-0.177333500459066,0.0485415758733555,
1.66642894980278));
#9956=CARTESIAN_POINT('Ctrl Pts',(-0.136948157917673,-0.12267296774877,
1.67754366268455));
#9957=CARTESIAN_POINT('Ctrl Pts',(0.0288064689070301,-0.181586459634089,
1.68865837556633));
#9958=CARTESIAN_POINT('Ctrl Pts',(0.168190194183902,-0.0742665035780993,
1.6997730884481));
#9959=CARTESIAN_POINT('Ctrl Pts',(0.153604091834597,0.101040773675795,1.71088780132988));
#9960=CARTESIAN_POINT('Ctrl Pts',(-0.00159898082742857,0.183850205965748,
1.72200251421165));
#9961=CARTESIAN_POINT('Ctrl Pts',(-0.155338265403761,0.098353842195845,
1.73311722709343));
#9962=CARTESIAN_POINT('Ctrl Pts',(-0.166873029294335,-0.0771806132877065,
1.74423193997521));
#9963=CARTESIAN_POINT('Ctrl Pts',(-0.025643765052489,-0.182060023858252,
1.75534665285698));
#9964=CARTESIAN_POINT('Ctrl Pts',(0.139061101343075,-0.120272461796479,
1.76646136573876));
#9965=CARTESIAN_POINT('Ctrl Pts',(0.176462387959855,0.0516186071958565,
1.77757607862053));
#9966=CARTESIAN_POINT('Ctrl Pts',(0.0523210615336027,0.176255387132795,
1.78869079150231));
#9967=CARTESIAN_POINT('Ctrl Pts',(-0.119717616249168,0.139539053074583,
1.79980550438409));
#9968=CARTESIAN_POINT('Ctrl Pts',(-0.182160720834928,-0.0249184020000041,
1.81092021726586));
#9969=CARTESIAN_POINT('Ctrl Pts',(-0.0778446696726029,-0.16656428902048,
1.82203493014764));
#9970=CARTESIAN_POINT('Ctrl Pts',(0.0977343372718058,-0.155728784402163,
1.83314964302942));
#9971=CARTESIAN_POINT('Ctrl Pts',(0.183842378706508,-0.00233125821546848,
1.84426435591119));
#9972=CARTESIAN_POINT('Ctrl Pts',(0.101651789551148,0.15320041988971,1.85537906879297));
#9973=CARTESIAN_POINT('Ctrl Pts',(-0.0735959994667044,0.168484669438591,
1.86649378167474));
#9974=CARTESIAN_POINT('Ctrl Pts',(-0.181470280731337,0.0295295137891618,
1.87760849455652));
#9975=CARTESIAN_POINT('Ctrl Pts',(-0.12321747011018,-0.136458455337079,
1.88872320743829));
#9976=CARTESIAN_POINT('Ctrl Pts',(0.0478348573047686,-0.177525438740387,
1.89983792032007));
#9977=CARTESIAN_POINT('Ctrl Pts',(0.175096732074868,-0.0560766385408066,
1.91095263320185));
#9978=CARTESIAN_POINT('Ctrl Pts',(0.142066184410422,0.116707558540133,1.92206734608362));
#9979=CARTESIAN_POINT('Ctrl Pts',(-0.0210189483701118,0.182651741800479,
1.9331820589654));
#9980=CARTESIAN_POINT('Ctrl Pts',(-0.16486227057344,0.0813872638359589,
1.94429677184718));
#9981=CARTESIAN_POINT('Ctrl Pts',(-0.157782315082607,-0.0943832401462696,
1.95541148472895));
#9982=CARTESIAN_POINT('Ctrl Pts',(-0.0062604319656806,-0.183750542760931,
1.96652619761073));
#9983=CARTESIAN_POINT('Ctrl Pts',(0.150992567850975,-0.10490328606436,1.9776409104925));
#9984=CARTESIAN_POINT('Ctrl Pts',(0.170019318761453,0.0699777551885857,
1.98875562337428));
#9985=CARTESIAN_POINT('Ctrl Pts',(0.0334017687074566,0.180797612872902,
1.99987033625606));
#9986=CARTESIAN_POINT('Ctrl Pts',(-0.133793453221103,0.126106172919867,
2.01098504913783));
#9987=CARTESIAN_POINT('Ctrl Pts',(-0.178507367426113,-0.0440292487783591,
2.02209976201961));
#9988=CARTESIAN_POINT('Ctrl Pts',(-0.0598065907447483,-0.173858064744653,
2.03321447490139));
#9989=CARTESIAN_POINT('Ctrl Pts',(0.113644170098336,-0.144528397126456,
2.04432918778316));
#9990=CARTESIAN_POINT('Ctrl Pts',(0.183059298154547,0.0171098899136208,
2.05544390066494));
#9991=CARTESIAN_POINT('Ctrl Pts',(0.0848926672411447,0.163084916597067,
2.06655861354672));
#9992=CARTESIAN_POINT('Ctrl Pts',(-0.0909890136144577,0.159763745495145,
2.07767332642849));
#9993=CARTESIAN_POINT('Ctrl Pts',(-0.183574740100876,0.0101867449437282,
2.08878803931027));
#9994=CARTESIAN_POINT('Ctrl Pts',(-0.108106845918033,-0.148715718183394,
2.09990275219204));
#9995=CARTESIAN_POINT('Ctrl Pts',(0.0663275338242693,-0.17147627599867,
2.11101746507382));
#9996=CARTESIAN_POINT('Ctrl Pts',(0.180042327710072,-0.0372587603217594,
2.1221321779556));
#9997=CARTESIAN_POINT('Ctrl Pts',(0.128937250118005,0.131067312760423,2.13324689083737));
#9998=CARTESIAN_POINT('Ctrl Pts',(-0.0402035204677608,0.179407725381376,
2.14436160371915));
#9999=CARTESIAN_POINT('Ctrl Pts',(-0.172539951470817,0.0635092135777934,
2.15547631660092));
#10000=CARTESIAN_POINT('Ctrl Pts',(-0.146924565505413,-0.110528850528984,
2.1665910294827));
#10001=CARTESIAN_POINT('Ctrl Pts',(0.013193011805229,-0.183383204120377,
2.17770574236448));
#10002=CARTESIAN_POINT('Ctrl Pts',(0.161233041383799,-0.0883592771818423,
2.18882045524625));
#10003=CARTESIAN_POINT('Ctrl Pts',(0.161672166186531,0.08755320703735,2.19993516812803));
#10004=CARTESIAN_POINT('Ctrl Pts',(0.0141084106240242,0.183315054230848,
2.2110498810098));
#10005=CARTESIAN_POINT('Ctrl Pts',(-0.146370925859051,0.111260999182195,
2.22216459389158));
#10006=CARTESIAN_POINT('Ctrl Pts',(-0.172854847713642,-0.0626469919088142,
2.23327930677336));
#10007=CARTESIAN_POINT('Ctrl Pts',(-0.0410987787696598,-0.179204792201909,
2.24439401965513));
#10008=CARTESIAN_POINT('Ctrl Pts',(0.128281379817428,-0.13170936649677,
2.25550873253691));
#10009=CARTESIAN_POINT('Ctrl Pts',(0.18022591070051,0.0363593415954858,
2.26662344541869));
#10010=CARTESIAN_POINT('Ctrl Pts',(0.0671831774557089,0.171143144838974,
2.27773815830046));
#10011=CARTESIAN_POINT('Ctrl Pts',(-0.107363712783848,0.149253308736201,
2.28885287118224));
#10012=CARTESIAN_POINT('Ctrl Pts',(-0.18362200020929,-0.0092695600841741,
2.29996758406402));
#10013=CARTESIAN_POINT('Ctrl Pts',(-0.0917880045327959,-0.15930852573796,
2.31108229694579));
#10014=CARTESIAN_POINT('Ctrl Pts',(0.0840821369721223,-0.163504736890904,
2.32219700982757));
#10015=CARTESIAN_POINT('Ctrl Pts',(0.182962573561233,-0.0180273813676558,
2.33331172270934));
#10016=CARTESIAN_POINT('Ctrl Pts',(0.114381487141248,0.143966386512752,
2.34442643559112));
#10017=CARTESIAN_POINT('Ctrl Pts',(-0.0589705282315283,0.174140844480832,
2.35554114847289));
#10018=CARTESIAN_POINT('Ctrl Pts',(-0.178222903013509,0.0449459198210797,
2.36665586135467));
#10019=CARTESIAN_POINT('Ctrl Pts',(-0.134542235007309,-0.125486577151581,
2.37777057423645));
#10020=CARTESIAN_POINT('Ctrl Pts',(0.0327466243405011,-0.180863000230457,
2.38888528711822));
#10021=CARTESIAN_POINT('Ctrl Pts',(0.123618421332056,-0.107657388085867,
2.39629509570608));
#10022=CARTESIAN_POINT('Ctrl Pts',(0.143545299885864,-0.0599211930845618,
2.4));
#10023=CARTESIAN_POINT('Ctrl Pts',(-0.0744392439309176,0.151537102412042,
-0.0153382721514717));
#10024=CARTESIAN_POINT('Ctrl Pts',(-0.124833124304749,0.126782225262728,
-0.0116333678575463));
#10025=CARTESIAN_POINT('Ctrl Pts',(-0.198113325344336,0.023478375100856,
-0.0042235592696955));
#10026=CARTESIAN_POINT('Ctrl Pts',(-0.127022615597461,-0.154083203796675,
0.00689115361208068));
#10027=CARTESIAN_POINT('Ctrl Pts',(0.0605160006134741,-0.190099104575569,
0.0180058664938568));
#10028=CARTESIAN_POINT('Ctrl Pts',(0.192570426897894,-0.0523344192653271,
0.0291205793756331));
#10029=CARTESIAN_POINT('Ctrl Pts',(0.148380465079886,0.133467648273019,
0.0402352922574092));
#10030=CARTESIAN_POINT('Ctrl Pts',(-0.0316677758679159,0.197019648453023,
0.0513500051391854));
#10031=CARTESIAN_POINT('Ctrl Pts',(-0.182713495011001,0.0802450866099659,
0.0624647180209616));
#10032=CARTESIAN_POINT('Ctrl Pts',(-0.166500451783044,-0.110008399741151,
0.0735794309027378));
#10033=CARTESIAN_POINT('Ctrl Pts',(0.00213892357312778,-0.199544894679597,
0.0846941437845138));
#10034=CARTESIAN_POINT('Ctrl Pts',(0.168818443031448,-0.106412993084556,
0.0958088566662903));
#10035=CARTESIAN_POINT('Ctrl Pts',(0.180953938029707,0.0841374430075943,
0.106923569548066));
#10036=CARTESIAN_POINT('Ctrl Pts',(0.0274345364643011,0.197662786947523,
0.118038282429843));
#10037=CARTESIAN_POINT('Ctrl Pts',(-0.151199572092017,0.130238340780269,
0.129152995311619));
#10038=CARTESIAN_POINT('Ctrl Pts',(-0.191418065222447,-0.0564132733576527,
0.140267708193395));
#10039=CARTESIAN_POINT('Ctrl Pts',(-0.0564026890847757,-0.191421112856703,
0.151382421075171));
#10040=CARTESIAN_POINT('Ctrl Pts',(0.130246529644629,-0.151192472290029,
0.162497133956947));
#10041=CARTESIAN_POINT('Ctrl Pts',(0.197661493952255,0.0274454765313785,
0.173611846838723));
#10042=CARTESIAN_POINT('Ctrl Pts',(0.0841270988654031,0.180958415399658,
0.1847265597205));
#10043=CARTESIAN_POINT('Ctrl Pts',(-0.106421500635976,0.168812865512893,
0.195841272602275));
#10044=CARTESIAN_POINT('Ctrl Pts',(-0.199546467880638,0.00212745487426852,
0.206955985484052));
#10045=CARTESIAN_POINT('Ctrl Pts',(-0.109996483918663,-0.16650553144729,
0.218070698365828));
#10046=CARTESIAN_POINT('Ctrl Pts',(0.0802498552478435,-0.182710918065531,
0.229185411247605));
#10047=CARTESIAN_POINT('Ctrl Pts',(0.19703141027762,-0.0316534693109011,
0.24030012412938));
#10048=CARTESIAN_POINT('Ctrl Pts',(0.133440426579246,0.14838116881846,0.251414837011157));
#10049=CARTESIAN_POINT('Ctrl Pts',(-0.0523086862487663,0.192580165391978,
0.262529549892933));
#10050=CARTESIAN_POINT('Ctrl Pts',(-0.190171776743541,0.0604815184392873,
0.273644262774709));
#10051=CARTESIAN_POINT('Ctrl Pts',(-0.153941984879862,-0.126984975601611,
0.284758975656486));
#10052=CARTESIAN_POINT('Ctrl Pts',(0.0232141016978955,-0.198202987432875,
0.295873688538261));
#10053=CARTESIAN_POINT('Ctrl Pts',(0.179118823100709,-0.0879759396258336,
0.306988401420038));
#10054=CARTESIAN_POINT('Ctrl Pts',(0.17104909609995,0.102788741917448,0.318103114301814));
#10055=CARTESIAN_POINT('Ctrl Pts',(0.00639235777248694,0.199455399788411,
0.32921782718359));
#10056=CARTESIAN_POINT('Ctrl Pts',(-0.164116268825541,0.113530476300182,
0.340332540065366));
#10057=CARTESIAN_POINT('Ctrl Pts',(-0.18438454553609,-0.0763259989099004,
0.351447252947142));
#10058=CARTESIAN_POINT('Ctrl Pts',(-0.0358578646641422,-0.196309786521245,
0.362561965828918));
#10059=CARTESIAN_POINT('Ctrl Pts',(0.14549492279625,-0.136581646580809,
0.373676678710695));
#10060=CARTESIAN_POINT('Ctrl Pts',(0.193654284253789,0.0481802545901155,
0.384791391592471));
#10061=CARTESIAN_POINT('Ctrl Pts',(0.0645326995164768,0.188835508936616,
0.395906104474247));
#10062=CARTESIAN_POINT('Ctrl Pts',(-0.123665388872078,0.156621168228757,
0.407020817356023));
#10063=CARTESIAN_POINT('Ctrl Pts',(-0.198653912931686,-0.0189721274282693,
0.418135530237799));
#10064=CARTESIAN_POINT('Ctrl Pts',(-0.0917845773237327,-0.177197376131055,
0.429250243119575));
#10065=CARTESIAN_POINT('Ctrl Pts',(0.0991090120039419,-0.173207166369719,
0.440364956001352));
#10066=CARTESIAN_POINT('Ctrl Pts',(0.199273188903667,-0.0106543383834273,
0.451479668883127));
#10067=CARTESIAN_POINT('Ctrl Pts',(0.117012589526199,0.161652010920368,
0.462594381764904));
#10068=CARTESIAN_POINT('Ctrl Pts',(-0.0723672644954619,0.185973916912209,
0.473709094646681));
#10069=CARTESIAN_POINT('Ctrl Pts',(-0.195498457028802,0.0400458742142447,
0.484823807528456));
#10070=CARTESIAN_POINT('Ctrl Pts',(-0.139660454146413,-0.142542191262248,
0.495938520410233));
#10071=CARTESIAN_POINT('Ctrl Pts',(0.0440298064461046,-0.19463991082649,
0.507053233292008));
#10072=CARTESIAN_POINT('Ctrl Pts',(0.187412950789573,-0.0685543916796767,
0.518167946173786));
#10073=CARTESIAN_POINT('Ctrl Pts',(0.159228781901736,0.120289291943693,
0.529282659055561));
#10074=CARTESIAN_POINT('Ctrl Pts',(-0.0147214836452785,0.19901406146679,
0.540397371937338));
#10075=CARTESIAN_POINT('Ctrl Pts',(-0.175194956979385,0.0955512731009747,
0.551512084819113));
#10076=CARTESIAN_POINT('Ctrl Pts',(-0.175286087823317,-0.0953839931949897,
0.56262679770089));
#10077=CARTESIAN_POINT('Ctrl Pts',(-0.0149114503840338,-0.19899991806448,
0.573741510582666));
#10078=CARTESIAN_POINT('Ctrl Pts',(0.159113884448319,-0.12044123263232,
0.584856223464442));
#10079=CARTESIAN_POINT('Ctrl Pts',(0.187478305573349,0.068375461106829,
0.595970936346218));
#10080=CARTESIAN_POINT('Ctrl Pts',(0.0442155843858271,0.194597792483998,
0.607085649227995));
#10081=CARTESIAN_POINT('Ctrl Pts',(-0.139524323591982,0.142675442415383,
0.618200362109771));
#10082=CARTESIAN_POINT('Ctrl Pts',(-0.195536594668278,-0.0398592384242233,
0.629315074991547));
#10083=CARTESIAN_POINT('Ctrl Pts',(-0.0725447572008543,-0.18590475234618,
0.640429787873323));
#10084=CARTESIAN_POINT('Ctrl Pts',(0.116858227572727,-0.16176363432733,
0.651544500755099));
#10085=CARTESIAN_POINT('Ctrl Pts',(0.19928326845738,0.010464112727274,0.662659213636875));
#10086=CARTESIAN_POINT('Ctrl Pts',(0.0992743057305387,0.173112480670647,
0.673773926518652));
#10087=CARTESIAN_POINT('Ctrl Pts',(-0.0916153876786538,0.177284910476655,
0.684888639400427));
#10088=CARTESIAN_POINT('Ctrl Pts',(-0.198635712143757,0.0191617484423541,
0.696003352282205));
#10089=CARTESIAN_POINT('Ctrl Pts',(-0.123814838864976,-0.156503049232485,
0.707118065163979));
#10090=CARTESIAN_POINT('Ctrl Pts',(0.0643524128403538,-0.188897024073568,
0.718232778045757));
#10091=CARTESIAN_POINT('Ctrl Pts',(0.193608204454711,-0.0483650897864192,
0.729347490927532));
#10092=CARTESIAN_POINT('Ctrl Pts',(0.145625233657563,0.136442698831435,
0.74046220380931));
#10093=CARTESIAN_POINT('Ctrl Pts',(-0.0356704563089337,0.196343926030162,
0.751576916691083));
#10094=CARTESIAN_POINT('Ctrl Pts',(-0.184311602793374,0.0765019726409902,
0.762691629572863));
#10095=CARTESIAN_POINT('Ctrl Pts',(-0.164224567178383,-0.113373763619712,
0.773806342454636));
#10096=CARTESIAN_POINT('Ctrl Pts',(0.00620196012416494,-0.199461410886526,
0.784921055336414));
#10097=CARTESIAN_POINT('Ctrl Pts',(0.170950898814037,-0.102951973933957,
0.796035768218188));
#10098=CARTESIAN_POINT('Ctrl Pts',(0.179202720946941,0.0878049175584046,
0.807150481099967));
#10099=CARTESIAN_POINT('Ctrl Pts',(0.0234032903405015,0.198180737569178,
0.818265193981741));
#10100=CARTESIAN_POINT('Ctrl Pts',(-0.153820698321162,0.127131866619725,
0.829379906863519));
#10101=CARTESIAN_POINT('Ctrl Pts',(-0.190229424114698,-0.0602999580697674,
0.840494619745293));
#10102=CARTESIAN_POINT('Ctrl Pts',(-0.0524924942563878,-0.192530145143477,
0.851609332627072));
#10103=CARTESIAN_POINT('Ctrl Pts',(0.13329872516108,-0.148508479935175,
0.862724045508846));
#10104=CARTESIAN_POINT('Ctrl Pts',(0.197061535993685,0.0314653742077725,
0.873838758390623));
#10105=CARTESIAN_POINT('Ctrl Pts',(0.0804242297093462,0.182634230137408,
0.884953471272399));
#10106=CARTESIAN_POINT('Ctrl Pts',(-0.109837492346678,0.166610455906041,
0.896068184154175));
#10107=CARTESIAN_POINT('Ctrl Pts',(-0.199548407350193,-0.00193697347089583,
0.907182897035951));
#10108=CARTESIAN_POINT('Ctrl Pts',(-0.106582597162507,-0.168711199166861,
0.918297609917728));
#10109=CARTESIAN_POINT('Ctrl Pts',(0.0839543240681803,-0.181038642870743,
0.929412322799503));
#10110=CARTESIAN_POINT('Ctrl Pts',(0.197635202246108,-0.027634137861807,
0.94052703568128));
#10111=CARTESIAN_POINT('Ctrl Pts',(0.130390800146249,0.151068057442487,
0.951641748563056));
#10112=CARTESIAN_POINT('Ctrl Pts',(-0.0562199486064098,0.191474896842688,
0.962756461444832));
#10113=CARTESIAN_POINT('Ctrl Pts',(-0.19136410718071,0.0565959117353481,
0.973871174326609));
#10114=CARTESIAN_POINT('Ctrl Pts',(-0.151323863718857,-0.130093839252372,
0.984985887208385));
#10115=CARTESIAN_POINT('Ctrl Pts',(0.0272459136767254,-0.197689096639511,
0.996100600090161));
#10116=CARTESIAN_POINT('Ctrl Pts',(0.180873400871156,-0.084309736089776,
1.00721531297194));
#10117=CARTESIAN_POINT('Ctrl Pts',(0.168920210253646,0.106251029689549,
1.01833002585371));
#10118=CARTESIAN_POINT('Ctrl Pts',(0.00232889830253915,0.199544218094441,
1.02944473873549));
#10119=CARTESIAN_POINT('Ctrl Pts',(-0.166394405183155,0.110164516365158,
1.04055945161727));
#10120=CARTESIAN_POINT('Ctrl Pts',(-0.18279183730445,-0.0800653667767086,
1.05167416449904));
#10121=CARTESIAN_POINT('Ctrl Pts',(-0.0318523576765106,-0.196999355462583,
1.06278887738082));
#10122=CARTESIAN_POINT('Ctrl Pts',(0.148246384444326,-0.133590150240991,
1.07390359026259));
#10123=CARTESIAN_POINT('Ctrl Pts',(0.192632873125826,0.0521142488530221,
1.08501830314437));
#10124=CARTESIAN_POINT('Ctrl Pts',(0.0606734671240232,0.190110623399576,
1.09613301602615));
#10125=CARTESIAN_POINT('Ctrl Pts',(-0.126829505611247,0.15407009848972,
1.10724772890792));
#10126=CARTESIAN_POINT('Ctrl Pts',(-0.198226321197279,-0.0230140028421487,
1.1183624417897));
#10127=CARTESIAN_POINT('Ctrl Pts',(-0.0881567162597448,-0.179029919623856,
1.12947715467147));
#10128=CARTESIAN_POINT('Ctrl Pts',(0.102616014519724,-0.171152774754934,
1.14059186755325));
#10129=CARTESIAN_POINT('Ctrl Pts',(0.199448845033595,-0.00659370586168438,
1.15170658043503));
#10130=CARTESIAN_POINT('Ctrl Pts',(0.113696094746692,0.164001575546019,
1.1628212933168));
#10131=CARTESIAN_POINT('Ctrl Pts',(-0.0761398227834604,0.184461503107637,
1.17393600619858));
#10132=CARTESIAN_POINT('Ctrl Pts',(-0.196273487775402,0.0360560222252062,
1.18505071908035));
#10133=CARTESIAN_POINT('Ctrl Pts',(-0.136728454927659,-0.145356968719496,
1.19616543196213));
#10134=CARTESIAN_POINT('Ctrl Pts',(0.0479847349517988,-0.193702823814809,
1.20728014484391));
#10135=CARTESIAN_POINT('Ctrl Pts',(0.188770266592525,-0.0647232971410789,
1.21839485772568));
#10136=CARTESIAN_POINT('Ctrl Pts',(0.156745929327229,0.123507215908905,
1.22950957060746));
#10137=CARTESIAN_POINT('Ctrl Pts',(-0.0187715755197026,0.198672964176643,
1.24062428348924));
#10138=CARTESIAN_POINT('Ctrl Pts',(-0.177104628793434,0.0919634123016617,
1.25173899637101));
#10139=CARTESIAN_POINT('Ctrl Pts',(-0.173307129216344,-0.09893410789518,
1.26285370925279));
#10140=CARTESIAN_POINT('Ctrl Pts',(-0.0108555003583793,-0.199262331749367,
1.27396842213457));
#10141=CARTESIAN_POINT('Ctrl Pts',(0.161533803683835,-0.117175718515645,
1.28508313501634));
#10142=CARTESIAN_POINT('Ctrl Pts',(0.186046877309155,0.0721794859065759,
1.29619784789812));
#10143=CARTESIAN_POINT('Ctrl Pts',(0.0402432105996758,0.195457930877352,
1.3073125607799));
#10144=CARTESIAN_POINT('Ctrl Pts',(-0.142401130616552,0.139804280125299,
1.31842727366167));
#10145=CARTESIAN_POINT('Ctrl Pts',(-0.194684259984547,-0.0438332939270479,
1.32954198654345));
#10146=CARTESIAN_POINT('Ctrl Pts',(-0.0687435511745859,-0.187343649249534,
1.34065669942522));
#10147=CARTESIAN_POINT('Ctrl Pts',(0.120128488300164,-0.159350133482664,
1.351771412307));
#10148=CARTESIAN_POINT('Ctrl Pts',(0.199028821479448,0.0145205703306567,
1.36288612518877));
#10149=CARTESIAN_POINT('Ctrl Pts',(0.0957280847061954,0.175098408161551,
1.37400083807055));
#10150=CARTESIAN_POINT('Ctrl Pts',(-0.0952069923014279,0.175382289183205,
1.38511555095233));
#10151=CARTESIAN_POINT('Ctrl Pts',(-0.19898476347094,0.0151123343213224,
1.3962302638341));
#10152=CARTESIAN_POINT('Ctrl Pts',(-0.120601797621762,-0.158992217270611,
1.40734497671588));
#10153=CARTESIAN_POINT('Ctrl Pts',(0.0681861658631651,-0.187547235455782,
1.41845968959766));
#10154=CARTESIAN_POINT('Ctrl Pts',(0.194553057445636,-0.0444120094206586,
1.42957440247943));
#10155=CARTESIAN_POINT('Ctrl Pts',(0.142816220303608,0.139380220836447,
1.44068911536121));
#10156=CARTESIAN_POINT('Ctrl Pts',(-0.0396618228229078,0.195576733157576,
1.45180382824298));
#10157=CARTESIAN_POINT('Ctrl Pts',(-0.18583142327823,0.0727323921276658,
1.46291854112476));
#10158=CARTESIAN_POINT('Ctrl Pts',(-0.161881520937861,-0.116694866729734,
1.47403325400654));
#10159=CARTESIAN_POINT('Ctrl Pts',(0.0102629298160299,-0.199293730493,1.48514796688831));
#10160=CARTESIAN_POINT('Ctrl Pts',(0.173012174491582,-0.09944901316715,
1.49626267977009));
#10161=CARTESIAN_POINT('Ctrl Pts',(0.177377306389596,0.0914363708826889,
1.50737739265186));
#10162=CARTESIAN_POINT('Ctrl Pts',(0.0193622625459762,0.198616267036026,
1.51849210553364));
#10163=CARTESIAN_POINT('Ctrl Pts',(-0.156377977710683,0.123972766482573,
1.52960681841542));
#10164=CARTESIAN_POINT('Ctrl Pts',(-0.188961891943262,-0.0641616874423405,
1.54072153129719));
#10165=CARTESIAN_POINT('Ctrl Pts',(-0.0485605137121908,-0.193559280971576,
1.55183624417897));
#10166=CARTESIAN_POINT('Ctrl Pts',(0.136295619815311,-0.145762899125208,
1.56295095706075));
#10167=CARTESIAN_POINT('Ctrl Pts',(0.196379835509003,0.0354722278364698,
1.57406566994252));
#10168=CARTESIAN_POINT('Ctrl Pts',(0.0766879972579736,0.184234279705994,
1.5851803828243));
#10169=CARTESIAN_POINT('Ctrl Pts',(-0.11320792022669,0.164338934949004,
1.59629509570607));
#10170=CARTESIAN_POINT('Ctrl Pts',(-0.199467570164373,-0.00600059954892135,
1.60740980858785));
#10171=CARTESIAN_POINT('Ctrl Pts',(-0.103124497367579,-0.170846881109693,
1.61852452146962));
#10172=CARTESIAN_POINT('Ctrl Pts',(0.0876239666636226,-0.179291269191664,
1.6296392343514));
#10173=CARTESIAN_POINT('Ctrl Pts',(0.198157010832902,-0.0236033429834524,
1.64075394723318));
#10174=CARTESIAN_POINT('Ctrl Pts',(0.127287084698812,0.153692279607998,
1.65186866011496));
#10175=CARTESIAN_POINT('Ctrl Pts',(-0.060107889671358,0.190290200329605,
1.66298337299673));
#10176=CARTESIAN_POINT('Ctrl Pts',(-0.192477055571666,0.0526868277721045,
1.67409808587851));
#10177=CARTESIAN_POINT('Ctrl Pts',(-0.148642970074574,-0.133148737093653,
1.68521279876028));
#10178=CARTESIAN_POINT('Ctrl Pts',(0.0312664234467219,-0.197093200052857,
1.69632751164206));
#10179=CARTESIAN_POINT('Ctrl Pts',(0.182552948364186,-0.0806085590106191,
1.70744222452384));
#10180=CARTESIAN_POINT('Ctrl Pts',(0.166721252575211,0.10966924218749,1.71855693740561));
#10181=CARTESIAN_POINT('Ctrl Pts',(-0.00173552724546146,0.199550261055719,
1.72967165028739));
#10182=CARTESIAN_POINT('Ctrl Pts',(-0.168603517469208,0.106752857756764,
1.74078636316916));
#10183=CARTESIAN_POINT('Ctrl Pts',(-0.181123302984206,-0.0837715217619741,
1.75190107605094));
#10184=CARTESIAN_POINT('Ctrl Pts',(-0.0278336376279517,-0.197607204723465,
1.76301578893272));
#10185=CARTESIAN_POINT('Ctrl Pts',(0.150936350220227,-0.130543237758309,
1.77413050181449));
#10186=CARTESIAN_POINT('Ctrl Pts',(0.191531553630485,0.0560266249752561,
1.78524521469627));
#10187=CARTESIAN_POINT('Ctrl Pts',(0.0567890660382895,0.191306875780052,
1.79635992757805));
#10188=CARTESIAN_POINT('Ctrl Pts',(-0.129941010672249,0.151455117073342,
1.80747464045982));
#10189=CARTESIAN_POINT('Ctrl Pts',(-0.197716500809795,-0.0270463315397067,
1.8185893533416));
#10190=CARTESIAN_POINT('Ctrl Pts',(-0.0844922858441475,-0.180788197554642,
1.82970406622337));
#10191=CARTESIAN_POINT('Ctrl Pts',(0.106080449647855,-0.169027385191674,
1.84081877910515));
#10192=CARTESIAN_POINT('Ctrl Pts',(0.199541765380578,-0.0025303381252174,
1.85193349198693));
#10193=CARTESIAN_POINT('Ctrl Pts',(0.1103324363177,0.166283108698467,1.8630482048687));
#10194=CARTESIAN_POINT('Ctrl Pts',(-0.0798807965924946,0.182872570600334,
1.87416291775048));
#10195=CARTESIAN_POINT('Ctrl Pts',(-0.196967099947332,0.0320512134023539,
1.88527763063225));
#10196=CARTESIAN_POINT('Ctrl Pts',(-0.133739737728071,-0.148111448897957,
1.89639234351403));
#10197=CARTESIAN_POINT('Ctrl Pts',(0.0519197583303703,-0.192685384596604,
1.90750705639581));
#10198=CARTESIAN_POINT('Ctrl Pts',(0.190049276322557,-0.0608653539503196,
1.91862176927758));
#10199=CARTESIAN_POINT('Ctrl Pts',(0.154198055081705,0.126673906355039,
1.92973648215936));
#10200=CARTESIAN_POINT('Ctrl Pts',(-0.0228138805302983,0.198249452956054,
1.94085119504114));
#10201=CARTESIAN_POINT('Ctrl Pts',(-0.178940833698592,0.0883374030492047,
1.95196590792291));
#10202=CARTESIAN_POINT('Ctrl Pts',(-0.17125627898712,-0.10244318254385,
1.96308062080469));
#10203=CARTESIAN_POINT('Ctrl Pts',(-0.00679504723157641,-0.199442087021132,
1.97419533368646));
#10204=CARTESIAN_POINT('Ctrl Pts',(0.163886715132369,-0.113861597324754,
1.98531004656824));
#10205=CARTESIAN_POINT('Ctrl Pts',(0.184538272694043,0.0759535690625106,
1.99642475945002));
#10206=CARTESIAN_POINT('Ctrl Pts',(0.0362541430415187,0.196236989007019,
2.00753947233179));
#10207=CARTESIAN_POINT('Ctrl Pts',(-0.145218866509139,0.136875123934236,
2.01865418521357));
#10208=CARTESIAN_POINT('Ctrl Pts',(-0.193751165973055,-0.0477891664121737,
2.02976889809535));
#10209=CARTESIAN_POINT('Ctrl Pts',(-0.0649138288057709,-0.188704831872211,
2.04088361097712));
#10210=CARTESIAN_POINT('Ctrl Pts',(0.123348917078771,-0.156870530685843,
2.0519983238589));
#10211=CARTESIAN_POINT('Ctrl Pts',(0.19869181295463,0.0185710044814121,
2.06311303674067));
#10212=CARTESIAN_POINT('Ctrl Pts',(0.0921421535575656,0.177011700967353,
2.07422774962245));
#10213=CARTESIAN_POINT('Ctrl Pts',(-0.0987591029588015,0.173406915446888,
2.08534246250422));
#10214=CARTESIAN_POINT('Ctrl Pts',(-0.19925127153347,0.0110566512675373,
2.09645717538601));
#10215=CARTESIAN_POINT('Ctrl Pts',(-0.11733872807775,-0.161415431822329,
2.10757188826778));
#10216=CARTESIAN_POINT('Ctrl Pts',(0.0719916337340498,-0.186119648115988,
2.11868660114956));
#10217=CARTESIAN_POINT('Ctrl Pts',(0.195417205582667,-0.0404405059530035,
2.12980131403133));
#10218=CARTESIAN_POINT('Ctrl Pts',(0.139947963537486,0.142259924811219,
2.14091602691311));
#10219=CARTESIAN_POINT('Ctrl Pts',(-0.043636736562569,0.194728410812529,
2.15203073979488));
#10220=CARTESIAN_POINT('Ctrl Pts',(-0.187274157119832,0.0689326404739108,
2.16314545267666));
#10221=CARTESIAN_POINT('Ctrl Pts',(-0.159471322036838,-0.11996756196921,
2.17426016555844));
#10222=CARTESIAN_POINT('Ctrl Pts',(0.0143196410143589,-0.199043379164193,
2.18537487844021));
#10223=CARTESIAN_POINT('Ctrl Pts',(0.175001683190603,-0.0959047977983527,
2.19648959132199));
#10224=CARTESIAN_POINT('Ctrl Pts',(0.175478307454146,0.0950298925627762,
2.20760430420376));
#10225=CARTESIAN_POINT('Ctrl Pts',(0.0153132111455397,0.198969409553037,
2.21871901708554));
#10226=CARTESIAN_POINT('Ctrl Pts',(-0.15887040383073,0.120762233120711,
2.22983372996731));
#10227=CARTESIAN_POINT('Ctrl Pts',(-0.18761594421292,-0.0679967886034852,
2.2409484428491));
#10228=CARTESIAN_POINT('Ctrl Pts',(-0.0446084462591464,-0.194508147970143,
2.25206315573087));
#10229=CARTESIAN_POINT('Ctrl Pts',(0.139236084597726,-0.142956807308717,
2.26317786861265));
#10230=CARTESIAN_POINT('Ctrl Pts',(0.195616465809081,0.0394642805488386,
2.27429258149442));
#10231=CARTESIAN_POINT('Ctrl Pts',(0.0729203458294538,0.185758068918763,
2.28540729437619));
#10232=CARTESIAN_POINT('Ctrl Pts',(-0.116532134415559,0.161998930407982,
2.29652200725798));
#10233=CARTESIAN_POINT('Ctrl Pts',(-0.199302567461706,-0.0100611425750267,
2.30763672013975));
#10234=CARTESIAN_POINT('Ctrl Pts',(-0.0996263244312855,-0.172912821785659,
2.31875143302153));
#10235=CARTESIAN_POINT('Ctrl Pts',(0.0912624073210796,-0.177467372195954,
2.3298661459033));
#10236=CARTESIAN_POINT('Ctrl Pts',(0.198586828476941,-0.0195668459503173,
2.34098085878508));
#10237=CARTESIAN_POINT('Ctrl Pts',(0.1241491979793,0.156260526666046,2.35209557166686));
#10238=CARTESIAN_POINT('Ctrl Pts',(-0.0640063699759371,0.189011759840439,
2.36321028454863));
#10239=CARTESIAN_POINT('Ctrl Pts',(-0.19344240946393,0.0487841174099963,
2.37432499743041));
#10240=CARTESIAN_POINT('Ctrl Pts',(-0.146031591195115,-0.136202617223352,
2.38543971031218));
#10241=CARTESIAN_POINT('Ctrl Pts',(0.0355430520271422,-0.196307960177277,
2.39655442319396));
#10242=CARTESIAN_POINT('Ctrl Pts',(0.134174928543208,-0.11685088838635,
2.40396423178181));
#10243=CARTESIAN_POINT('Ctrl Pts',(0.155803480964729,-0.0650382177163376,
2.40766913607574));
#10244=CARTESIAN_POINT('Ctrl Pts',(-0.0802959149489801,0.163459616787401,
-0.00766913607573617));
#10245=CARTESIAN_POINT('Ctrl Pts',(-0.134654644548669,0.136757095305608,
-0.00396423178181077));
#10246=CARTESIAN_POINT('Ctrl Pts',(-0.213700326361063,0.0253255878308996,
0.00344557680604003));
#10247=CARTESIAN_POINT('Ctrl Pts',(-0.13701639887793,-0.166206038290849,
0.0145602896878162));
#10248=CARTESIAN_POINT('Ctrl Pts',(0.0652772298818827,-0.205055569170507,
0.0256750025695924));
#10249=CARTESIAN_POINT('Ctrl Pts',(0.207721328204669,-0.0564519446507592,
0.0367897154513685));
#10250=CARTESIAN_POINT('Ctrl Pts',(0.160054624079751,0.143968508655411,
0.0479044283331447));
#10251=CARTESIAN_POINT('Ctrl Pts',(-0.0341593076908942,0.212520602038122,
0.059019141214921));
#10252=CARTESIAN_POINT('Ctrl Pts',(-0.197088880551355,0.0865585450530169,
0.070133854096697));
#10253=CARTESIAN_POINT('Ctrl Pts',(-0.179600240536358,-0.118663552218321,
0.0812485669784734));
#10254=CARTESIAN_POINT('Ctrl Pts',(0.00230720808327818,-0.21524452755814,
0.0923632798602493));
#10255=CARTESIAN_POINT('Ctrl Pts',(0.182100604837577,-0.114785269045894,
0.103477992742026));
#10256=CARTESIAN_POINT('Ctrl Pts',(0.195190886559782,0.0907571411395873,
0.114592705623802));
#10257=CARTESIAN_POINT('Ctrl Pts',(0.0295930088791093,0.213214340866297,
0.125707418505578));
#10258=CARTESIAN_POINT('Ctrl Pts',(-0.163095530528085,0.140485128302662,
0.136822131387354));
#10259=CARTESIAN_POINT('Ctrl Pts',(-0.206478301943304,-0.0608517115477897,
0.14793684426913));
#10260=CARTESIAN_POINT('Ctrl Pts',(-0.0608402945339887,-0.206481589356881,
0.159051557150907));
#10261=CARTESIAN_POINT('Ctrl Pts',(0.140493961443918,-0.163087872133576,
0.170166270032683));
#10262=CARTESIAN_POINT('Ctrl Pts',(0.213212946141786,0.0296048096800013,
0.181280982914459));
#10263=CARTESIAN_POINT('Ctrl Pts',(0.0907459831492815,0.195195716196652,
0.192395695796235));
#10264=CARTESIAN_POINT('Ctrl Pts',(-0.114794445947616,0.182094588495495,
0.203510408678011));
#10265=CARTESIAN_POINT('Ctrl Pts',(-0.215246224534229,0.00229483705933785,
0.214625121559788));
#10266=CARTESIAN_POINT('Ctrl Pts',(-0.11865069889232,-0.179605719854349,
0.225739834441564));
#10267=CARTESIAN_POINT('Ctrl Pts',(0.0865636888739609,-0.197086100859037,
0.23685454732334));
#10268=CARTESIAN_POINT('Ctrl Pts',(0.212533289250105,-0.0341438755340746,
0.247969260205116));
#10269=CARTESIAN_POINT('Ctrl Pts',(0.143939145235083,0.160055383186509,
0.259083973086892));
#10270=CARTESIAN_POINT('Ctrl Pts',(-0.0564241870326071,0.207731832896163,
0.270198685968668));
#10271=CARTESIAN_POINT('Ctrl Pts',(-0.205133958980916,0.0652400347468957,
0.281313398850444));
#10272=CARTESIAN_POINT('Ctrl Pts',(-0.16605370866557,-0.136975797472738,
0.292428111732221));
#10273=CARTESIAN_POINT('Ctrl Pts',(0.025040522137507,-0.213797042811354,
0.303542824613997));
#10274=CARTESIAN_POINT('Ctrl Pts',(0.193211389933017,-0.0948976399103106,
0.314657537495773));
#10275=CARTESIAN_POINT('Ctrl Pts',(0.184506759435748,0.110875871957748,
0.325772250377549));
#10276=CARTESIAN_POINT('Ctrl Pts',(0.00689529056070297,0.215147991459819,
0.336886963259325));
#10277=CARTESIAN_POINT('Ctrl Pts',(-0.177028476747947,0.122462735886679,
0.348001676141102));
#10278=CARTESIAN_POINT('Ctrl Pts',(-0.198891404646875,-0.082331114520091,
0.359116389022878));
#10279=CARTESIAN_POINT('Ctrl Pts',(-0.0386790609264599,-0.211754890159689,
0.370231101904654));
#10280=CARTESIAN_POINT('Ctrl Pts',(0.156942055419018,-0.14732750761979,
0.38134581478643));
#10281=CARTESIAN_POINT('Ctrl Pts',(0.208890460418672,0.0519709419453341,
0.392460527668207));
#10282=CARTESIAN_POINT('Ctrl Pts',(0.0696099513935343,0.203692557369242,
0.403575240549982));
#10283=CARTESIAN_POINT('Ctrl Pts',(-0.133395034965965,0.168943682649122,
0.414689953431759));
#10284=CARTESIAN_POINT('Ctrl Pts',(-0.214283445864218,-0.0204648012249496,
0.425804666313535));
#10285=CARTESIAN_POINT('Ctrl Pts',(-0.0990059305445593,-0.191138768902671,
0.436919379195311));
#10286=CARTESIAN_POINT('Ctrl Pts',(0.106906631210968,-0.186834620624077,
0.448034092077087));
#10287=CARTESIAN_POINT('Ctrl Pts',(0.214951444733503,-0.0114925918574203,
0.459148804958863));
#10288=CARTESIAN_POINT('Ctrl Pts',(0.126218812019027,0.174370337939476,
0.47026351784064));
#10289=CARTESIAN_POINT('Ctrl Pts',(-0.0780609179804491,0.200605823306979,
0.481378230722416));
#10290=CARTESIAN_POINT('Ctrl Pts',(-0.210879727537387,0.0431965713266546,
0.492492943604192));
#10291=CARTESIAN_POINT('Ctrl Pts',(-0.150648547133053,-0.153757011246062,
0.503607656485968));
#10292=CARTESIAN_POINT('Ctrl Pts',(0.0474939481773568,-0.209953633326855,
0.514722369367745));
#10293=CARTESIAN_POINT('Ctrl Pts',(0.202158076335407,-0.0739480590211045,
0.52583708224952));
#10294=CARTESIAN_POINT('Ctrl Pts',(0.171756456055305,0.129753316196324,
0.536951795131297));
#10295=CARTESIAN_POINT('Ctrl Pts',(-0.0158797287060216,0.214671929876368,
0.548066508013073));
#10296=CARTESIAN_POINT('Ctrl Pts',(-0.188978805026037,0.103068979385421,
0.55918122089485));
#10297=CARTESIAN_POINT('Ctrl Pts',(-0.189077105789276,-0.102888538365418,
0.570295933776625));
#10298=CARTESIAN_POINT('Ctrl Pts',(-0.0160846414951921,-0.214656673710818,
0.581410646658403));
#10299=CARTESIAN_POINT('Ctrl Pts',(0.171632518792379,-0.129917211152352,
0.592525359540176));
#10300=CARTESIAN_POINT('Ctrl Pts',(0.202228573050342,0.073755050692434,
0.603640072421955));
#10301=CARTESIAN_POINT('Ctrl Pts',(0.0476943426045303,0.20990820123126,
0.614754785303729));
#10302=CARTESIAN_POINT('Ctrl Pts',(-0.150501706208254,0.153900746226344,
0.625869498185507));
#10303=CARTESIAN_POINT('Ctrl Pts',(-0.210920865739414,-0.0429952515559257,
0.636984211067282));
#10304=CARTESIAN_POINT('Ctrl Pts',(-0.0782523753142842,-0.200531217066804,
0.64809892394906));
#10305=CARTESIAN_POINT('Ctrl Pts',(0.126052305299824,-0.17449074356315,
0.659213636830834));
#10306=CARTESIAN_POINT('Ctrl Pts',(0.214962317318242,0.011287399779957,
0.670328349712612));
#10307=CARTESIAN_POINT('Ctrl Pts',(0.107084929784557,0.186732485319662,
0.681443062594386));
#10308=CARTESIAN_POINT('Ctrl Pts',(-0.0988234295325455,0.191233190205171,
0.692557775476164));
#10309=CARTESIAN_POINT('Ctrl Pts',(-0.214263813089322,0.0206693410888018,
0.703672488357938));
#10310=CARTESIAN_POINT('Ctrl Pts',(-0.133556243265307,-0.168816270381381,
0.714787201239717));
#10311=CARTESIAN_POINT('Ctrl Pts',(0.069415480267185,-0.203758912344705,
0.72590191412149));
#10312=CARTESIAN_POINT('Ctrl Pts',(0.208840755190191,-0.0521703194566796,
0.73701662700327));
#10313=CARTESIAN_POINT('Ctrl Pts',(0.15708261877356,0.147177627851049,0.748131339885043));
#10314=CARTESIAN_POINT('Ctrl Pts',(-0.0384769078072813,0.211791715669455,
0.759246052766822));
#10315=CARTESIAN_POINT('Ctrl Pts',(-0.198812722973664,0.0825209333709834,
0.770360765648595));
#10316=CARTESIAN_POINT('Ctrl Pts',(-0.177145295711566,-0.122293693491868,
0.781475478530374));
#10317=CARTESIAN_POINT('Ctrl Pts',(0.0066899129592092,-0.215154475494282,
0.792590191412148));
#10318=CARTESIAN_POINT('Ctrl Pts',(0.184400836262686,-0.111051946611679,
0.803704904293927));
#10319=CARTESIAN_POINT('Ctrl Pts',(0.193301888626575,0.094713162306093,
0.8148196171757));
#10320=CARTESIAN_POINT('Ctrl Pts',(0.0252445956121046,0.213773042390762,
0.825934330057479));
#10321=CARTESIAN_POINT('Ctrl Pts',(-0.16592287962047,0.137134245464334,
0.837049042939253));
#10322=CARTESIAN_POINT('Ctrl Pts',(-0.205196141885616,-0.0650441897165239,
0.848163755821031));
#10323=CARTESIAN_POINT('Ctrl Pts',(-0.0566224565389448,-0.207677877194747,
0.859278468702805));
#10324=CARTESIAN_POINT('Ctrl Pts',(0.143786295146609,-0.160192710784959,
0.870393181584584));
#10325=CARTESIAN_POINT('Ctrl Pts',(0.212565785173049,0.0339409816355746,
0.881507894466357));
#10326=CARTESIAN_POINT('Ctrl Pts',(0.0867517826292189,0.197003379339731,
0.892622607348135));
#10327=CARTESIAN_POINT('Ctrl Pts',(-0.118479198309198,0.179718899475349,
0.903737320229911));
#10328=CARTESIAN_POINT('Ctrl Pts',(-0.21524831659581,-0.0020893691131805,
0.914852033111686));
#10329=CARTESIAN_POINT('Ctrl Pts',(-0.114968217097204,-0.181984923326388,
0.925966745993464));
#10330=CARTESIAN_POINT('Ctrl Pts',(0.0905596149154041,-0.195282255740236,
0.937081458875238));
#10331=CARTESIAN_POINT('Ctrl Pts',(0.21318458587791,-0.0298083143549778,
0.948196171757016));
#10332=CARTESIAN_POINT('Ctrl Pts',(0.140649582744129,0.162953668674638,
0.959310884638791));
#10333=CARTESIAN_POINT('Ctrl Pts',(-0.0606431765471154,0.206539604916095,
0.970425597520568));
#10334=CARTESIAN_POINT('Ctrl Pts',(-0.206420098634119,0.061048719400998,
0.981540310402345));
#10335=CARTESIAN_POINT('Ctrl Pts',(-0.163229601071661,-0.140329257799675,
0.99265502328412));
#10336=CARTESIAN_POINT('Ctrl Pts',(0.0293895457794294,-0.213242720531089,
1.0037697361659));
#10337=CARTESIAN_POINT('Ctrl Pts',(0.195104012963389,-0.0909429897584348,
1.01488444904767));
#10338=CARTESIAN_POINT('Ctrl Pts',(0.182210378819503,0.114610562825048,
1.02599916192945));
#10339=CARTESIAN_POINT('Ctrl Pts',(0.00251212949178726,0.215243797741161,
1.03711387481123));
#10340=CARTESIAN_POINT('Ctrl Pts',(-0.179485850487301,0.118831951660617,
1.048228587693));
#10341=CARTESIAN_POINT('Ctrl Pts',(-0.197173386596812,-0.0863646853671406,
1.05934330057478));
#10342=CARTESIAN_POINT('Ctrl Pts',(-0.034358411878696,-0.212498712452088,
1.07045801345655));
#10343=CARTESIAN_POINT('Ctrl Pts',(0.159909994355694,-0.144100648734776,
1.08157272633833));
#10344=CARTESIAN_POINT('Ctrl Pts',(0.207788687526742,0.0562144518476816,
1.0926874392201));
#10345=CARTESIAN_POINT('Ctrl Pts',(0.0654470854160082,0.205067994263295,
1.10380215210188));
#10346=CARTESIAN_POINT('Ctrl Pts',(-0.136808095539401,0.166191901895078,
1.11491686498366));
#10347=CARTESIAN_POINT('Ctrl Pts',(-0.213822212410925,-0.0248246800647778,
1.12603157786543));
#10348=CARTESIAN_POINT('Ctrl Pts',(-0.095092639542961,-0.193115491779851,
1.13714629074721));
#10349=CARTESIAN_POINT('Ctrl Pts',(0.110689554852622,-0.184618595236638,
1.14826100362899));
#10350=CARTESIAN_POINT('Ctrl Pts',(0.215140920995271,-0.00711248015306863,
1.15937571651076));
#10351=CARTESIAN_POINT('Ctrl Pts',(0.12264138472824,0.176904759722742,1.17049042939254));
#10352=CARTESIAN_POINT('Ctrl Pts',(-0.0821302905779772,0.198974417024396,
1.18160514227431));
#10353=CARTESIAN_POINT('Ctrl Pts',(-0.211715735530289,0.0388928089688832,
1.19271985515609));
#10354=CARTESIAN_POINT('Ctrl Pts',(-0.147485866435784,-0.156793247502267,
1.20383456803787));
#10355=CARTESIAN_POINT('Ctrl Pts',(0.0517600393700242,-0.20894281893627,
1.21494928091964));
#10356=CARTESIAN_POINT('Ctrl Pts',(0.203622181940428,-0.0698155447048894,
1.22606399380142));
#10357=CARTESIAN_POINT('Ctrl Pts',(0.169078259601047,0.133224417397496,
1.2371787066832));
#10358=CARTESIAN_POINT('Ctrl Pts',(-0.0202484704544748,0.214303996007717,
1.24829341956497));
#10359=CARTESIAN_POINT('Ctrl Pts',(-0.191038724464548,0.0991988357571789,
1.25940813244675));
#10360=CARTESIAN_POINT('Ctrl Pts',(-0.186942448267222,-0.106717966137282,
1.27052284532852));
#10361=CARTESIAN_POINT('Ctrl Pts',(-0.0117095806925935,-0.214939733368739,
1.2816375582103));
#10362=CARTESIAN_POINT('Ctrl Pts',(0.174242830488972,-0.126394775540022,
1.29275227109208));
#10363=CARTESIAN_POINT('Ctrl Pts',(0.200684524023408,0.077858365498637,
1.30386698397385));
#10364=CARTESIAN_POINT('Ctrl Pts',(0.0434094335856485,0.210836012901957,
1.31498169685563));
#10365=CARTESIAN_POINT('Ctrl Pts',(-0.153604852344235,0.150803688936734,
1.32609640973741));
#10366=CARTESIAN_POINT('Ctrl Pts',(-0.210001471752333,-0.0472819746042342,
1.33721112261918));
#10367=CARTESIAN_POINT('Ctrl Pts',(-0.0741521010547544,-0.202083322344489,
1.34832583550096));
#10368=CARTESIAN_POINT('Ctrl Pts',(0.129579860972944,-0.171887355238405,
1.35944054838274));
#10369=CARTESIAN_POINT('Ctrl Pts',(0.214687851165442,0.0156630080950769,
1.37055526126451));
#10370=CARTESIAN_POINT('Ctrl Pts',(0.10325970203204,0.188874660017895,1.38166997414629));
#10371=CARTESIAN_POINT('Ctrl Pts',(-0.102697611537783,0.189180876002454,
1.39278468702806));
#10372=CARTESIAN_POINT('Ctrl Pts',(-0.214640326796344,0.0163013304174776,
1.40389939990984));
#10373=CARTESIAN_POINT('Ctrl Pts',(-0.130090408945011,-0.17150127918223,
1.41501411279161));
#10374=CARTESIAN_POINT('Ctrl Pts',(0.0735508622296984,-0.202302926142676,
1.42612882567339));
#10375=CARTESIAN_POINT('Ctrl Pts',(0.209859946565495,-0.0479062218104144,
1.43724353855517));
#10376=CARTESIAN_POINT('Ctrl Pts',(0.154052600124136,0.150346265851913,
1.44835825143694));
#10377=CARTESIAN_POINT('Ctrl Pts',(-0.0427823038485639,0.21096416221252,
1.45947296431872));
#10378=CARTESIAN_POINT('Ctrl Pts',(-0.20045211867337,0.0784547728310926,
1.4705876772005));
#10379=CARTESIAN_POINT('Ctrl Pts',(-0.174617905161696,-0.125876091683695,
1.48170239008227));
#10380=CARTESIAN_POINT('Ctrl Pts',(0.0110703883612833,-0.214973602477494,
1.49281710296405));
#10381=CARTESIAN_POINT('Ctrl Pts',(0.186624287331642,-0.107273382712479,
1.50393181584582));
#10382=CARTESIAN_POINT('Ctrl Pts',(0.191332855569507,0.0986303281969572,
1.5150465287276));
#10383=CARTESIAN_POINT('Ctrl Pts',(0.0208856310799447,0.214242838095031,
1.52616124160938));
#10384=CARTESIAN_POINT('Ctrl Pts',(-0.168681358582888,0.133726596185098,
1.53727595449115));
#10385=CARTESIAN_POINT('Ctrl Pts',(-0.203828883836526,-0.0692097491295648,
1.54839066737293));
#10386=CARTESIAN_POINT('Ctrl Pts',(-0.0523811187890492,-0.208787982544563,
1.55950538025471));
#10387=CARTESIAN_POINT('Ctrl Pts',(0.14701897707028,-0.157231115374246,
1.57062009313648));
#10388=CARTESIAN_POINT('Ctrl Pts',(0.211830450405416,0.0382630832743479,
1.58173480601826));
#10389=CARTESIAN_POINT('Ctrl Pts',(0.082721593883301,0.198729316322549,
1.59284951890003));
#10390=CARTESIAN_POINT('Ctrl Pts',(-0.122114802005634,0.177268661617743,
1.60396423178181));
#10391=CARTESIAN_POINT('Ctrl Pts',(-0.215161119366841,-0.0064727098984307,
1.61507894466359));
#10392=CARTESIAN_POINT('Ctrl Pts',(-0.11123804370538,-0.184288634736983,
1.62619365754536));
#10393=CARTESIAN_POINT('Ctrl Pts',(0.0945179747022152,-0.193397403598943,
1.63730837042714));
#10394=CARTESIAN_POINT('Ctrl Pts',(0.213747448901395,-0.0254603878361445,
1.64842308330892));
#10395=CARTESIAN_POINT('Ctrl Pts',(0.137301675666721,0.165784357282983,
1.65953779619069));
#10396=CARTESIAN_POINT('Ctrl Pts',(-0.0648370099150017,0.205261699802723,
1.67065250907247));
#10397=CARTESIAN_POINT('Ctrl Pts',(-0.207620610684265,0.0568320796708535,
1.68176722195424));
#10398=CARTESIAN_POINT('Ctrl Pts',(-0.160337782231475,-0.143624506438537,
1.69288193483602));
#10399=CARTESIAN_POINT('Ctrl Pts',(0.0337263779864135,-0.212599940471626,
1.7039966477178));
#10400=CARTESIAN_POINT('Ctrl Pts',(0.196915702544469,-0.0869506144431389,
1.71511136059957));
#10401=CARTESIAN_POINT('Ctrl Pts',(0.179838413315825,0.118297710699184,
1.72622607348135));
#10402=CARTESIAN_POINT('Ctrl Pts',(-0.00187207366349427,0.21525031614569,
1.73734078636313));
#10403=CARTESIAN_POINT('Ctrl Pts',(-0.181868769534656,0.115151873317682,
1.7484554992449));
#10404=CARTESIAN_POINT('Ctrl Pts',(-0.195373576674077,-0.0903624302362419,
1.75957021212668));
#10405=CARTESIAN_POINT('Ctrl Pts',(-0.0300235102034143,-0.213154385588678,
1.77068492500845));
#10406=CARTESIAN_POINT('Ctrl Pts',(0.162811599097379,-0.140814013720139,
1.78179963789023));
#10407=CARTESIAN_POINT('Ctrl Pts',(0.206600719301116,0.0604346427546558,
1.792914350772));
#10408=CARTESIAN_POINT('Ctrl Pts',(0.0612570705429762,0.206358364427309,
1.80402906365378));
#10409=CARTESIAN_POINT('Ctrl Pts',(-0.140164405095331,0.163371181072101,
1.81514377653556));
#10410=CARTESIAN_POINT('Ctrl Pts',(-0.213272280784662,-0.0291742610794093,
1.82625848941733));
#10411=CARTESIAN_POINT('Ctrl Pts',(-0.0911399020156923,-0.195012106088805,
1.83737320229911));
#10412=CARTESIAN_POINT('Ctrl Pts',(0.114426562023903,-0.182325985981184,
1.84848791518088));
#10413=CARTESIAN_POINT('Ctrl Pts',(0.215241152054647,-0.00272941803496647,
1.85960262806266));
#10414=CARTESIAN_POINT('Ctrl Pts',(0.119013083084253,0.179365797507223,
1.87071734094444));
#10415=CARTESIAN_POINT('Ctrl Pts',(-0.0861655937182851,0.197260471762076,
1.88183205382621));
#10416=CARTESIAN_POINT('Ctrl Pts',(-0.212463919163327,0.034572913015546,
1.89294676670799));
#10417=CARTESIAN_POINT('Ctrl Pts',(-0.144262005345963,-0.159764442458836,
1.90406147958977));
#10418=CARTESIAN_POINT('Ctrl Pts',(0.056004659355972,-0.207845330452822,
1.91517619247154));
#10419=CARTESIAN_POINT('Ctrl Pts',(0.205001820570246,-0.0656540693598324,
1.92629090535332));
#10420=CARTESIAN_POINT('Ctrl Pts',(0.166329925752987,0.136640254169945,
1.9374056182351));
#10421=CARTESIAN_POINT('Ctrl Pts',(-0.0246088126904845,0.213847164111628,
1.94852033111687));
#10422=CARTESIAN_POINT('Ctrl Pts',(-0.193019396823745,0.0952875422624504,
1.95963504399865));
#10423=CARTESIAN_POINT('Ctrl Pts',(-0.184730242891633,-0.110503124941429,
1.97074975688042));
#10424=CARTESIAN_POINT('Ctrl Pts',(-0.0073296624974724,-0.215133631281334,
1.9818644697622));
#10425=CARTESIAN_POINT('Ctrl Pts',(0.176780862413764,-0.122819908585148,
1.99297918264398));
#10426=CARTESIAN_POINT('Ctrl Pts',(0.199057226626634,0.0819293829364356,
2.00409389552575));
#10427=CARTESIAN_POINT('Ctrl Pts',(0.0391065173755809,0.211676365141135,
2.01520860840753));
#10428=CARTESIAN_POINT('Ctrl Pts',(-0.156644279797176,0.147644074948605,
2.02632332128931));
#10429=CARTESIAN_POINT('Ctrl Pts',(-0.208994964519996,-0.0515490840459884,
2.03743803417108));
#10430=CARTESIAN_POINT('Ctrl Pts',(-0.0700210668667938,-0.20355159899977,
2.04855274705286));
#10431=CARTESIAN_POINT('Ctrl Pts',(0.133053664059207,-0.16921266424523,
2.05966745993463));
#10432=CARTESIAN_POINT('Ctrl Pts',(0.214324327754712,0.0200321190492036,
2.07078217281641));
#10433=CARTESIAN_POINT('Ctrl Pts',(0.0993916398739864,0.190938485337639,
2.08189688569819));
#10434=CARTESIAN_POINT('Ctrl Pts',(-0.106529192303145,0.18705008539863,
2.09301159857996));
#10435=CARTESIAN_POINT('Ctrl Pts',(-0.214927802966064,0.0119265575913465,
2.10412631146174));
#10436=CARTESIAN_POINT('Ctrl Pts',(-0.126570610237467,-0.174115145461265,
2.11524102434351));
#10437=CARTESIAN_POINT('Ctrl Pts',(0.0776557336438302,-0.200763020233305,
2.12635573722529));
#10438=CARTESIAN_POINT('Ctrl Pts',(0.210792083455263,-0.0436222515842479,
2.13747045010707));
#10439=CARTESIAN_POINT('Ctrl Pts',(0.150958676956968,0.153452536862016,
2.14858516298884));
#10440=CARTESIAN_POINT('Ctrl Pts',(-0.0470699526573771,0.210049096243681,
2.15969987587062));
#10441=CARTESIAN_POINT('Ctrl Pts',(-0.202008362768847,0.0743560673700281,
2.17081458875239));
#10442=CARTESIAN_POINT('Ctrl Pts',(-0.172018078568263,-0.129406273409436,
2.18192930163417));
#10443=CARTESIAN_POINT('Ctrl Pts',(0.0154462702234889,-0.214703554208009,
2.19304401451595));
#10444=CARTESIAN_POINT('Ctrl Pts',(0.188770324997408,-0.103450318414863,
2.20415872739772));
#10445=CARTESIAN_POINT('Ctrl Pts',(0.18928444872176,0.102506578088203,2.2152734402795));
#10446=CARTESIAN_POINT('Ctrl Pts',(0.0165180116670554,0.214623764875225,
2.22638815316127));
#10447=CARTESIAN_POINT('Ctrl Pts',(-0.171369881802411,0.130263467059228,
2.23750286604305));
#10448=CARTESIAN_POINT('Ctrl Pts',(-0.202377040712198,-0.073346585298156,
2.24861757892483));
#10449=CARTESIAN_POINT('Ctrl Pts',(-0.0481181137486331,-0.209811503738378,
2.2597322918066));
#10450=CARTESIAN_POINT('Ctrl Pts',(0.150190789378024,-0.154204248120663,
2.27084700468838));
#10451=CARTESIAN_POINT('Ctrl Pts',(0.211007020917653,0.0425692195021916,
2.28196171757016));
#10452=CARTESIAN_POINT('Ctrl Pts',(0.0786575142031988,0.200372992998553,
2.29307643045193));
#10453=CARTESIAN_POINT('Ctrl Pts',(-0.12570055604727,0.174744552079762,
2.30419114333371));
#10454=CARTESIAN_POINT('Ctrl Pts',(-0.214983134714123,-0.0108527250658792,
2.31530585621548));
#10455=CARTESIAN_POINT('Ctrl Pts',(-0.107464644329775,-0.186517117833358,
2.32642056909726));
#10456=CARTESIAN_POINT('Ctrl Pts',(0.0984426776700368,-0.191430007501004,
2.33753528197904));
#10457=CARTESIAN_POINT('Ctrl Pts',(0.214211083392649,-0.0211063105329791,
2.34864999486081));
#10458=CARTESIAN_POINT('Ctrl Pts',(0.133916908817353,0.168554666819339,
2.35976470774259));
#10459=CARTESIAN_POINT('Ctrl Pts',(-0.0690422117203459,0.203882675200046,
2.37087942062436));
#10460=CARTESIAN_POINT('Ctrl Pts',(-0.208661915914351,0.0526223149989132,
2.38199413350615));
#10461=CARTESIAN_POINT('Ctrl Pts',(-0.157520947382922,-0.146918657295124,
2.39310884638792));
#10462=CARTESIAN_POINT('Ctrl Pts',(0.0383394797137831,-0.211752920124096,
2.4042235592697));
#10463=CARTESIAN_POINT('Ctrl Pts',(0.144731435754359,-0.126044388686833,
2.41163336785755));
#10464=CARTESIAN_POINT('Ctrl Pts',(0.168061662043594,-0.0701552423481134,
2.41533827215147));
#10465=CARTESIAN_POINT('Ctrl Pts',(-0.0861525859670425,0.175382131162759,
-6.38378239159465E-16));
#10466=CARTESIAN_POINT('Ctrl Pts',(-0.14447616479259,0.146731965348487,
0.00370490429392476));
#10467=CARTESIAN_POINT('Ctrl Pts',(-0.22928732737779,0.0271728005609432,
0.0111147128817755));
#10468=CARTESIAN_POINT('Ctrl Pts',(-0.147010182158398,-0.178328872785022,
0.0222294257635518));
#10469=CARTESIAN_POINT('Ctrl Pts',(0.0700384591502911,-0.220012033765444,
0.0333441386453279));
#10470=CARTESIAN_POINT('Ctrl Pts',(0.222872229511445,-0.0605694700361912,
0.0444588515271041));
#10471=CARTESIAN_POINT('Ctrl Pts',(0.171728783079617,0.154469369037803,
0.0555735644088802));
#10472=CARTESIAN_POINT('Ctrl Pts',(-0.0366508395138724,0.228021555623221,
0.0666882772906566));
#10473=CARTESIAN_POINT('Ctrl Pts',(-0.211464266091708,0.0928720034960677,
0.0778029901724325));
#10474=CARTESIAN_POINT('Ctrl Pts',(-0.192700029289671,-0.127318704695491,
0.0889177030542089));
#10475=CARTESIAN_POINT('Ctrl Pts',(0.00247549259342858,-0.230944160436682,
0.100032415935985));
#10476=CARTESIAN_POINT('Ctrl Pts',(0.195382766643706,-0.123157545007232,
0.111147128817761));
#10477=CARTESIAN_POINT('Ctrl Pts',(0.209427835089857,0.0973768392715804,
0.122261841699537));
#10478=CARTESIAN_POINT('Ctrl Pts',(0.0317514812939175,0.228765894785071,
0.133376554581313));
#10479=CARTESIAN_POINT('Ctrl Pts',(-0.174991488964152,0.150731915825055,
0.14449126746309));
#10480=CARTESIAN_POINT('Ctrl Pts',(-0.221538538664161,-0.0652901497379268,
0.155605980344866));
#10481=CARTESIAN_POINT('Ctrl Pts',(-0.0652778999832015,-0.221542065857059,
0.166720693226642));
#10482=CARTESIAN_POINT('Ctrl Pts',(0.150741393243207,-0.174983271977123,
0.177835406108418));
#10483=CARTESIAN_POINT('Ctrl Pts',(0.228764398331316,0.0317641428286243,
0.188950118990194));
#10484=CARTESIAN_POINT('Ctrl Pts',(0.0973648674331599,0.209433016993645,
0.200064831871971));
#10485=CARTESIAN_POINT('Ctrl Pts',(-0.123167391259255,0.195376311478096,
0.211179544753747));
#10486=CARTESIAN_POINT('Ctrl Pts',(-0.230945981187819,0.00246221924440694,
0.222294257635523));
#10487=CARTESIAN_POINT('Ctrl Pts',(-0.127304913865976,-0.192705908261409,
0.233408970517299));
#10488=CARTESIAN_POINT('Ctrl Pts',(0.0928775225000782,-0.211461283652542,
0.244523683399076));
#10489=CARTESIAN_POINT('Ctrl Pts',(0.228035168222589,-0.0366342817572481,
0.255638396280851));
#10490=CARTESIAN_POINT('Ctrl Pts',(0.15443786389092,0.171729597554559,0.266753109162628));
#10491=CARTESIAN_POINT('Ctrl Pts',(-0.0605396878164478,0.222883500400348,
0.277867822044404));
#10492=CARTESIAN_POINT('Ctrl Pts',(-0.220096141218292,0.0699985510545042,
0.28898253492618));
#10493=CARTESIAN_POINT('Ctrl Pts',(-0.178165432451279,-0.146966619343865,
0.300097247807956));
#10494=CARTESIAN_POINT('Ctrl Pts',(0.0268669425771186,-0.229391098189834,
0.311211960689733));
#10495=CARTESIAN_POINT('Ctrl Pts',(0.207303956765325,-0.101819340194788,
0.322326673571508));
#10496=CARTESIAN_POINT('Ctrl Pts',(0.197964422771547,0.118963001998048,
0.333441386453285));
#10497=CARTESIAN_POINT('Ctrl Pts',(0.00739822334891944,0.230840583131227,
0.344556099335061));
#10498=CARTESIAN_POINT('Ctrl Pts',(-0.189940684670355,0.131394995473175,
0.355670812216837));
#10499=CARTESIAN_POINT('Ctrl Pts',(-0.213398263757659,-0.0883362301302812,
0.366785525098613));
#10500=CARTESIAN_POINT('Ctrl Pts',(-0.0415002571887781,-0.227199993798133,
0.37790023798039));
#10501=CARTESIAN_POINT('Ctrl Pts',(0.168389188041786,-0.158073368658771,
0.389014950862165));
#10502=CARTESIAN_POINT('Ctrl Pts',(0.224126636583554,0.0557616293005522,
0.400129663743942));
#10503=CARTESIAN_POINT('Ctrl Pts',(0.074687203270592,0.218549605801867,
0.411244376625718));
#10504=CARTESIAN_POINT('Ctrl Pts',(-0.143124681059852,0.181266197069486,
0.422359089507494));
#10505=CARTESIAN_POINT('Ctrl Pts',(-0.22991297879675,-0.0219574750216296,
0.433473802389271));
#10506=CARTESIAN_POINT('Ctrl Pts',(-0.106227283765387,-0.205080161674287,
0.444588515271047));
#10507=CARTESIAN_POINT('Ctrl Pts',(0.114704250417995,-0.200462074878434,
0.455703228152823));
#10508=CARTESIAN_POINT('Ctrl Pts',(0.230629700563337,-0.0123308453314138,
0.466817941034599));
#10509=CARTESIAN_POINT('Ctrl Pts',(0.135425034511855,0.187088664958583,
0.477932653916375));
#10510=CARTESIAN_POINT('Ctrl Pts',(-0.0837545714654364,0.215237729701748,
0.489047366798152));
#10511=CARTESIAN_POINT('Ctrl Pts',(-0.226260998045971,0.0463472684390648,
0.500162079679927));
#10512=CARTESIAN_POINT('Ctrl Pts',(-0.161636640119692,-0.164971831229877,
0.511276792561705));
#10513=CARTESIAN_POINT('Ctrl Pts',(0.0509580899086091,-0.225267355827221,
0.522391505443479));
#10514=CARTESIAN_POINT('Ctrl Pts',(0.216903201881242,-0.0793417263625324,
0.533506218325257));
#10515=CARTESIAN_POINT('Ctrl Pts',(0.184284130208874,0.139217340448956,
0.544620931207032));
#10516=CARTESIAN_POINT('Ctrl Pts',(-0.0170379737667647,0.230329798285947,
0.555735644088809));
#10517=CARTESIAN_POINT('Ctrl Pts',(-0.202762653072689,0.110586685669867,
0.566850356970584));
#10518=CARTESIAN_POINT('Ctrl Pts',(-0.202868123755235,-0.110393083535847,
0.577965069852361));
#10519=CARTESIAN_POINT('Ctrl Pts',(-0.0172578326063502,-0.230313429357155,
0.589079782734137));
#10520=CARTESIAN_POINT('Ctrl Pts',(0.18415115313644,-0.139393189672384,
0.600194495615913));
#10521=CARTESIAN_POINT('Ctrl Pts',(0.216978840527336,0.0791346402780395,
0.61130920849769));
#10522=CARTESIAN_POINT('Ctrl Pts',(0.0511731008232336,0.225218609978521,
0.622423921379465));
#10523=CARTESIAN_POINT('Ctrl Pts',(-0.161479088824527,0.165126050037305,
0.633538634261242));
#10524=CARTESIAN_POINT('Ctrl Pts',(-0.22630513681055,-0.0461312646876283,
0.644653347143017));
#10525=CARTESIAN_POINT('Ctrl Pts',(-0.0839599934277138,-0.215157681787428,
0.655768060024794));
#10526=CARTESIAN_POINT('Ctrl Pts',(0.135246383026922,-0.18721785279897,
0.66688277290657));
#10527=CARTESIAN_POINT('Ctrl Pts',(0.230641366179104,0.01211068683264,0.677997485788347));
#10528=CARTESIAN_POINT('Ctrl Pts',(0.114895553838575,0.200352489968677,
0.689112198670123));
#10529=CARTESIAN_POINT('Ctrl Pts',(-0.106031471386437,0.205181469933688,
0.700226911551899));
#10530=CARTESIAN_POINT('Ctrl Pts',(-0.229891914034888,0.0221769337352497,
0.711341624433676));
#10531=CARTESIAN_POINT('Ctrl Pts',(-0.143297647665638,-0.181129491530277,
0.722456337315451));
#10532=CARTESIAN_POINT('Ctrl Pts',(0.0744785476940164,-0.218620800615842,
0.733571050197228));
#10533=CARTESIAN_POINT('Ctrl Pts',(0.224073305925671,-0.0559755491269399,
0.744685763079003));
#10534=CARTESIAN_POINT('Ctrl Pts',(0.168540003889557,0.157912556870662,
0.75580047596078));
#10535=CARTESIAN_POINT('Ctrl Pts',(-0.0412833593056288,0.227239505308747,
0.766915188842556));
#10536=CARTESIAN_POINT('Ctrl Pts',(-0.213313843153954,0.0885398941009765,
0.778029901724332));
#10537=CARTESIAN_POINT('Ctrl Pts',(-0.19006602424475,-0.131213623364024,
0.789144614606108));
#10538=CARTESIAN_POINT('Ctrl Pts',(0.00717786579425366,-0.230847540102037,
0.800259327487884));
#10539=CARTESIAN_POINT('Ctrl Pts',(0.197850773711335,-0.119151919289402,
0.811374040369661));
#10540=CARTESIAN_POINT('Ctrl Pts',(0.207401056306209,0.101621407053782,
0.822488753251437));
#10541=CARTESIAN_POINT('Ctrl Pts',(0.0270859008837078,0.229365347212345,
0.833603466133214));
#10542=CARTESIAN_POINT('Ctrl Pts',(-0.178025060919778,0.147136624308943,
0.844718179014988));
#10543=CARTESIAN_POINT('Ctrl Pts',(-0.220162859656535,-0.0697884213632804,
0.855832891896766));
#10544=CARTESIAN_POINT('Ctrl Pts',(-0.0607524188215016,-0.222825609246017,
0.86694760477854));
#10545=CARTESIAN_POINT('Ctrl Pts',(0.154273865132138,-0.171876941634742,
0.878062317660319));
#10546=CARTESIAN_POINT('Ctrl Pts',(0.228070034352413,0.0364165890633767,
0.889177030542093));
#10547=CARTESIAN_POINT('Ctrl Pts',(0.0930793355490916,0.211372528542054,
0.900291743423871));
#10548=CARTESIAN_POINT('Ctrl Pts',(-0.127120904271719,0.192827343044658,
0.911406456305645));
#10549=CARTESIAN_POINT('Ctrl Pts',(-0.230948225841428,-0.00224176475546543,
0.922521169187423));
#10550=CARTESIAN_POINT('Ctrl Pts',(-0.123353837031902,-0.195258647485915,
0.933635882069198));
#10551=CARTESIAN_POINT('Ctrl Pts',(0.0971649057626279,-0.209525868609729,
0.944750594950976));
#10552=CARTESIAN_POINT('Ctrl Pts',(0.228733969509712,-0.0319824908481486,
0.95586530783275));
#10553=CARTESIAN_POINT('Ctrl Pts',(0.15090836534201,0.174839279906789,0.966980020714528));
#10554=CARTESIAN_POINT('Ctrl Pts',(-0.0650664044878212,0.221604312989502,
0.978094733596303));
#10555=CARTESIAN_POINT('Ctrl Pts',(-0.221476090087528,0.0655015270666479,
0.98920944647808));
#10556=CARTESIAN_POINT('Ctrl Pts',(-0.175135338424465,-0.150564676346977,
1.00032415935986));
#10557=CARTESIAN_POINT('Ctrl Pts',(0.0315331778821334,-0.228796344422667,
1.01143887224163));
#10558=CARTESIAN_POINT('Ctrl Pts',(0.209334625055623,-0.0975762434270938,
1.02255358512341));
#10559=CARTESIAN_POINT('Ctrl Pts',(0.19550054738536,0.122970095960548,1.03366829800518));
#10560=CARTESIAN_POINT('Ctrl Pts',(0.00269536068103519,0.230943377387881,
1.04478301088696));
#10561=CARTESIAN_POINT('Ctrl Pts',(-0.192577295791447,0.127499386956076,
1.05589772376874));
#10562=CARTESIAN_POINT('Ctrl Pts',(-0.211554935889174,-0.0926640039575724,
1.06701243665051));
#10563=CARTESIAN_POINT('Ctrl Pts',(-0.0368644660808813,-0.227998069441593,
1.07812714953229));
#10564=CARTESIAN_POINT('Ctrl Pts',(0.171573604267061,-0.154611147228561,
1.08924186241407));
#10565=CARTESIAN_POINT('Ctrl Pts',(0.222944501927657,0.0603146548423409,
1.10035657529584));
#10566=CARTESIAN_POINT('Ctrl Pts',(0.0702207037079931,0.220025365127014,
1.11147128817762));
#10567=CARTESIAN_POINT('Ctrl Pts',(-0.146786685467554,0.178313705300437,
1.12258600105939));
#10568=CARTESIAN_POINT('Ctrl Pts',(-0.22941810362457,-0.0266353572874071,
1.13370071394117));
#10569=CARTESIAN_POINT('Ctrl Pts',(-0.102028562826177,-0.207201063935846,
1.14481542682294));
#10570=CARTESIAN_POINT('Ctrl Pts',(0.11876309518552,-0.198084415718342,
1.15593013970472));
#10571=CARTESIAN_POINT('Ctrl Pts',(0.230832996956947,-0.00763125444445281,
1.1670448525865));
#10572=CARTESIAN_POINT('Ctrl Pts',(0.131586674709788,0.189807943899465,
1.17815956546828));
#10573=CARTESIAN_POINT('Ctrl Pts',(-0.0881207583724943,0.213487330941155,
1.18927427835005));
#10574=CARTESIAN_POINT('Ctrl Pts',(-0.227157983285175,0.0417295957125604,
1.20038899123183));
#10575=CARTESIAN_POINT('Ctrl Pts',(-0.15824327794391,-0.168229526285038,
1.2115037041136));
#10576=CARTESIAN_POINT('Ctrl Pts',(0.0555353437882497,-0.22418281405773,
1.22261841699538));
#10577=CARTESIAN_POINT('Ctrl Pts',(0.218474097288331,-0.0749077922687001,
1.23373312987716));
#10578=CARTESIAN_POINT('Ctrl Pts',(0.181410589874865,0.142941618886087,
1.24484784275893));
#10579=CARTESIAN_POINT('Ctrl Pts',(-0.0217253653892473,0.229935027838791,
1.25596255564071));
#10580=CARTESIAN_POINT('Ctrl Pts',(-0.204972820135662,0.106434259212696,
1.26707726852249));
#10581=CARTESIAN_POINT('Ctrl Pts',(-0.200577767318102,-0.114501824379384,
1.27819198140426));
#10582=CARTESIAN_POINT('Ctrl Pts',(-0.0125636610268072,-0.230617134988113,
1.28930669428604));
#10583=CARTESIAN_POINT('Ctrl Pts',(0.186951857294109,-0.135613832564399,
1.30042140716781));
#10584=CARTESIAN_POINT('Ctrl Pts',(0.215322170737661,0.0835372450906981,
1.31153612004959));
#10585=CARTESIAN_POINT('Ctrl Pts',(0.046575656571621,0.226214094926563,
1.32265083293136));
#10586=CARTESIAN_POINT('Ctrl Pts',(-0.164808574071917,0.161803097748168,
1.33376554581314));
#10587=CARTESIAN_POINT('Ctrl Pts',(-0.225318683520119,-0.0507306552814204,
1.34488025869492));
#10588=CARTESIAN_POINT('Ctrl Pts',(-0.0795606509349228,-0.216822995439444,
1.35599497157669));
#10589=CARTESIAN_POINT('Ctrl Pts',(0.139031233645724,-0.184424576994146,
1.36710968445847));
#10590=CARTESIAN_POINT('Ctrl Pts',(0.230346880851436,0.0168054458594967,
1.37822439734025));
#10591=CARTESIAN_POINT('Ctrl Pts',(0.110791319357884,0.202650911874241,
1.38933911022202));
#10592=CARTESIAN_POINT('Ctrl Pts',(-0.110188230774137,0.202979462821703,
1.4004538231038));
#10593=CARTESIAN_POINT('Ctrl Pts',(-0.230295890121748,0.0174903265136328,
1.41156853598557));
#10594=CARTESIAN_POINT('Ctrl Pts',(-0.139579020268259,-0.184010341093849,
1.42268324886735));
#10595=CARTESIAN_POINT('Ctrl Pts',(0.0789155585962315,-0.217058616829571,
1.43379796174913));
#10596=CARTESIAN_POINT('Ctrl Pts',(0.225166835685355,-0.05140043420017,
1.4449126746309));
#10597=CARTESIAN_POINT('Ctrl Pts',(0.165288979944664,0.16131231086738,1.45602738751268));
#10598=CARTESIAN_POINT('Ctrl Pts',(-0.0459027848742203,0.226351591267464,
1.46714210039445));
#10599=CARTESIAN_POINT('Ctrl Pts',(-0.21507281406851,0.0841771535345191,
1.47825681327623));
#10600=CARTESIAN_POINT('Ctrl Pts',(-0.187354289385532,-0.135057316637657,
1.48937152615801));
#10601=CARTESIAN_POINT('Ctrl Pts',(0.0118778469065368,-0.230653474461988,
1.50048623903978));
#10602=CARTESIAN_POINT('Ctrl Pts',(0.200236400171702,-0.115097752257808,
1.51160095192156));
#10603=CARTESIAN_POINT('Ctrl Pts',(0.205288404749417,0.105824285511226,
1.52271566480333));
#10604=CARTESIAN_POINT('Ctrl Pts',(0.0224089996139133,0.229869409154036,
1.53383037768511));
#10605=CARTESIAN_POINT('Ctrl Pts',(-0.180984739455093,0.143480425887623,
1.54494509056689));
#10606=CARTESIAN_POINT('Ctrl Pts',(-0.21869587572979,-0.0742578108167894,
1.55605980344866));
#10607=CARTESIAN_POINT('Ctrl Pts',(-0.0562017238659076,-0.22401668411755,
1.56717451633044));
#10608=CARTESIAN_POINT('Ctrl Pts',(0.157742334325249,-0.168699331623285,
1.57828922921222));
#10609=CARTESIAN_POINT('Ctrl Pts',(0.22728106530183,0.0410539387122264,
1.58940394209399));
#10610=CARTESIAN_POINT('Ctrl Pts',(0.0887551905086285,0.213224352939102,
1.60051865497577));
#10611=CARTESIAN_POINT('Ctrl Pts',(-0.131021683784578,0.190198388286483,
1.61163336785754));
#10612=CARTESIAN_POINT('Ctrl Pts',(-0.230854668569309,-0.00694482024794042,
1.62274808073932));
#10613=CARTESIAN_POINT('Ctrl Pts',(-0.119351590043181,-0.197730388364273,
1.6338627936211));
#10614=CARTESIAN_POINT('Ctrl Pts',(0.101411982740808,-0.207503538006223,
1.64497750650287));
#10615=CARTESIAN_POINT('Ctrl Pts',(0.229337886969887,-0.0273174326888366,
1.65609221938465));
#10616=CARTESIAN_POINT('Ctrl Pts',(0.14731626663463,0.177876434957968,1.66720693226643));
#10617=CARTESIAN_POINT('Ctrl Pts',(-0.0695661301586456,0.220233199275841,
1.6783216451482));
#10618=CARTESIAN_POINT('Ctrl Pts',(-0.222764165796864,0.0609773315696025,
1.68943635802998));
#10619=CARTESIAN_POINT('Ctrl Pts',(-0.172032594388376,-0.154100275783421,
1.70055107091176));
#10620=CARTESIAN_POINT('Ctrl Pts',(0.0361863325261053,-0.228106680890394,
1.71166578379353));
#10621=CARTESIAN_POINT('Ctrl Pts',(0.211278456724753,-0.0932926698756588,
1.72278049667531));
#10622=CARTESIAN_POINT('Ctrl Pts',(0.192955574056439,0.126926179210878,
1.73389520955708));
#10623=CARTESIAN_POINT('Ctrl Pts',(-0.00200862008152737,0.230950371235661,
1.74500992243886));
#10624=CARTESIAN_POINT('Ctrl Pts',(-0.195134021600103,0.123550888878601,
1.75612463532063));
#10625=CARTESIAN_POINT('Ctrl Pts',(-0.209623850363949,-0.0969533387105092,
1.76723934820241));
#10626=CARTESIAN_POINT('Ctrl Pts',(-0.0322133827788769,-0.228701566453891,
1.77835406108419));
#10627=CARTESIAN_POINT('Ctrl Pts',(0.174686847974531,-0.151084789681969,
1.78946877396597));
#10628=CARTESIAN_POINT('Ctrl Pts',(0.221669884971746,0.0648426605340554,
1.80058348684774));
#10629=CARTESIAN_POINT('Ctrl Pts',(0.0657250750476629,0.221409853074566,
1.81169819972952));
#10630=CARTESIAN_POINT('Ctrl Pts',(-0.150387799518412,0.17528724507086,
1.82281291261129));
#10631=CARTESIAN_POINT('Ctrl Pts',(-0.228828060759529,-0.0313021906191119,
1.83392762549307));
#10632=CARTESIAN_POINT('Ctrl Pts',(-0.0977875181872369,-0.209236014622967,
1.84504233837484));
#10633=CARTESIAN_POINT('Ctrl Pts',(0.122772674399952,-0.195624586770695,
1.85615705125662));
#10634=CARTESIAN_POINT('Ctrl Pts',(0.230940538728716,-0.00292849794471524,
1.8672717641384));
#10635=CARTESIAN_POINT('Ctrl Pts',(0.127693729850804,0.192448486315979,
1.87838647702018));
#10636=CARTESIAN_POINT('Ctrl Pts',(-0.0924503908440751,0.211648372923818,
1.88950118990195));
#10637=CARTESIAN_POINT('Ctrl Pts',(-0.227960738379322,0.037094612628738,
1.90061590278373));
#10638=CARTESIAN_POINT('Ctrl Pts',(-0.154784272963854,-0.171417436019714,
1.9117306156655));
#10639=CARTESIAN_POINT('Ctrl Pts',(0.0600895603815735,-0.22300527630904,
1.92284532854728));
#10640=CARTESIAN_POINT('Ctrl Pts',(0.219954364817935,-0.0704427847693452,
1.93396004142905));
#10641=CARTESIAN_POINT('Ctrl Pts',(0.17846179642427,0.146606601984851,1.94507475431083));
#10642=CARTESIAN_POINT('Ctrl Pts',(-0.0264037448506712,0.229444875267203,
1.95618946719261));
#10643=CARTESIAN_POINT('Ctrl Pts',(-0.207097959948898,0.102237681475696,
1.96730418007438));
#10644=CARTESIAN_POINT('Ctrl Pts',(-0.198204206796146,-0.118563067339009,
1.97841889295616));
#10645=CARTESIAN_POINT('Ctrl Pts',(-0.00786427776336803,-0.230825175541536,
1.98953360583794));
#10646=CARTESIAN_POINT('Ctrl Pts',(0.189675009695157,-0.131778219845543,
2.00064831871971));
#10647=CARTESIAN_POINT('Ctrl Pts',(0.213576180559224,0.0879051968103603,
2.01176303160149));
#10648=CARTESIAN_POINT('Ctrl Pts',(0.041958891709643,0.227115741275252,
2.02287774448326));
#10649=CARTESIAN_POINT('Ctrl Pts',(-0.168069693085213,0.158413025962974,
2.03399245736504));
#10650=CARTESIAN_POINT('Ctrl Pts',(-0.224238763066937,-0.0553090016798028,
2.04510717024682));
#10651=CARTESIAN_POINT('Ctrl Pts',(-0.0751283049278165,-0.218398366127328,
2.05622188312859));
#10652=CARTESIAN_POINT('Ctrl Pts',(0.142758411039642,-0.181554797804617,
2.06733659601037));
#10653=CARTESIAN_POINT('Ctrl Pts',(0.229956842554795,0.0214932336169949,
2.07845130889215));
#10654=CARTESIAN_POINT('Ctrl Pts',(0.106641126190407,0.204865269707925,
2.08956602177392));
#10655=CARTESIAN_POINT('Ctrl Pts',(-0.114299281647489,0.200693255350372,
2.1006807346557));
#10656=CARTESIAN_POINT('Ctrl Pts',(-0.230604334398658,0.0127964639151555,
2.11179544753747));
#10657=CARTESIAN_POINT('Ctrl Pts',(-0.135802492397184,-0.186814859100201,
2.12291016041925));
#10658=CARTESIAN_POINT('Ctrl Pts',(0.0833198335536108,-0.215406392350623,
2.13402487330102));
#10659=CARTESIAN_POINT('Ctrl Pts',(0.226166961327859,-0.046803997215492,
2.1451395861828));
#10660=CARTESIAN_POINT('Ctrl Pts',(0.161969390376449,0.164645148912813,
2.15625429906458));
#10661=CARTESIAN_POINT('Ctrl Pts',(-0.0505031687521857,0.225369781674834,
2.16736901194636));
#10662=CARTESIAN_POINT('Ctrl Pts',(-0.216742568417862,0.0797794942661454,
2.17848372482813));
#10663=CARTESIAN_POINT('Ctrl Pts',(-0.184564835099688,-0.138844984849663,
2.18959843770991));
#10664=CARTESIAN_POINT('Ctrl Pts',(0.0165728994326188,-0.230363729251825,
2.20071315059168));
#10665=CARTESIAN_POINT('Ctrl Pts',(0.202538966804212,-0.110995839031374,
2.21182786347346));
#10666=CARTESIAN_POINT('Ctrl Pts',(0.203090589989375,0.109983263613629,
2.22294257635523));
#10667=CARTESIAN_POINT('Ctrl Pts',(0.017722812188571,0.230278120197415,
2.23405728923701));
#10668=CARTESIAN_POINT('Ctrl Pts',(-0.18386935977409,0.139764700997745,
2.24517200211879));
#10669=CARTESIAN_POINT('Ctrl Pts',(-0.217138137211476,-0.0786963819928267,
2.25628671500057));
#10670=CARTESIAN_POINT('Ctrl Pts',(-0.0516277812381195,-0.225114859506612,
2.26740142788234));
#10671=CARTESIAN_POINT('Ctrl Pts',(0.161145494158321,-0.165451688932609,
2.27851614076412));
#10672=CARTESIAN_POINT('Ctrl Pts',(0.226397576026225,0.0456741584555444,
2.28963085364589));
#10673=CARTESIAN_POINT('Ctrl Pts',(0.0843946825769435,0.214987917078343,
2.30074556652767));
#10674=CARTESIAN_POINT('Ctrl Pts',(-0.134868977678981,0.187490173751543,
2.31186027940945));
#10675=CARTESIAN_POINT('Ctrl Pts',(-0.23066370196654,-0.0116443075567319,
2.32297499229122));
#10676=CARTESIAN_POINT('Ctrl Pts',(-0.115302964228264,-0.200121413881057,
2.334089705173));
#10677=CARTESIAN_POINT('Ctrl Pts',(0.105622948018994,-0.205392642806054,
2.34520441805477));
#10678=CARTESIAN_POINT('Ctrl Pts',(0.229835338308358,-0.0226457751156407,
2.35631913093655));
#10679=CARTESIAN_POINT('Ctrl Pts',(0.143684619655405,0.180848806972633,
2.36743384381833));
#10680=CARTESIAN_POINT('Ctrl Pts',(-0.0740780534647546,0.218753590559653,
2.3785485567001));
#10681=CARTESIAN_POINT('Ctrl Pts',(-0.223881422364772,0.0564605125878301,
2.38966326958188));
#10682=CARTESIAN_POINT('Ctrl Pts',(-0.169010303570728,-0.157634697366895,
2.40077798246365));
#10683=CARTESIAN_POINT('Ctrl Pts',(0.041135907400424,-0.227197880070916,
2.41189269534543));
#10684=CARTESIAN_POINT('Ctrl Pts',(0.15528794296551,-0.135237888987316,
2.41930250393328));
#10685=CARTESIAN_POINT('Ctrl Pts',(0.180319843122459,-0.0752722669798892,
2.42300740822721));
#10686=CARTESIAN_POINT('',(-0.152020725150953,-0.123272996449671,2.4));
#10687=CARTESIAN_POINT('Ctrl Pts',(-0.152022961461291,-0.123275749177759,
2.4));
#10688=CARTESIAN_POINT('Ctrl Pts',(-0.148843860776273,-0.126520593760054,
2.4));
#10689=CARTESIAN_POINT('Ctrl Pts',(-0.145550280466061,-0.129639743170448,
2.4));
#10690=CARTESIAN_POINT('Ctrl Pts',(-0.142144069729337,-0.132625074476751,
2.4));
#10691=CARTESIAN_POINT('Ctrl Pts',(-0.132568315892317,-0.141017625590188,
2.4));
#10692=CARTESIAN_POINT('Ctrl Pts',(-0.122103883881501,-0.148356196379371,
2.4));
#10693=CARTESIAN_POINT('Ctrl Pts',(-0.110956607971893,-0.154597350195316,
2.4));
#10694=CARTESIAN_POINT('Ctrl Pts',(-0.105501670740442,-0.15765146876149,
2.4));
#10695=CARTESIAN_POINT('Ctrl Pts',(-0.0998828881521222,-0.160442052175162,
2.4));
#10696=CARTESIAN_POINT('Ctrl Pts',(-0.0941236483875527,-0.162959592659121,
2.4));
#10697=CARTESIAN_POINT('Ctrl Pts',(-0.090759079960923,-0.164430348795582,
2.4));
#10698=CARTESIAN_POINT('Ctrl Pts',(-0.0873466982488509,-0.165807525926122,
2.4));
#10699=CARTESIAN_POINT('Ctrl Pts',(-0.0839043527287597,-0.167084756767954,
2.4));
#10700=CARTESIAN_POINT('Ctrl Pts',(-0.0722464129819429,-0.171410261023684,
2.4));
#10701=CARTESIAN_POINT('Ctrl Pts',(-0.0602078660333974,-0.174610335907723,
2.4));
#10702=CARTESIAN_POINT('Ctrl Pts',(-0.047979011447792,-0.17663071349189,
2.4));
#10703=CARTESIAN_POINT('Ctrl Pts',(-0.0395067434511661,-0.178030450501403,
2.4));
#10704=CARTESIAN_POINT('Ctrl Pts',(-0.0309428099130652,-0.178862922405498,
2.4));
#10705=CARTESIAN_POINT('Ctrl Pts',(-0.0223535667019919,-0.179095476400577,
2.4));
#10706=CARTESIAN_POINT('Ctrl Pts',(-0.0183635027663534,-0.179203507490867,
2.4));
#10707=CARTESIAN_POINT('Ctrl Pts',(-0.014376249181295,-0.179181530851919,
2.4));
#10708=CARTESIAN_POINT('Ctrl Pts',(-0.0104054136088075,-0.179027692656729,
2.4));
#10709=CARTESIAN_POINT('Ctrl Pts',(0.00121824750065017,-0.178577368533774,
2.4));
#10710=CARTESIAN_POINT('Ctrl Pts',(0.0127220893604508,-0.17700119131334,
2.4));
#10711=CARTESIAN_POINT('Ctrl Pts',(0.0239367001203737,-0.17422702409659,
2.4));
#10712=CARTESIAN_POINT('Ctrl Pts',(0.0263036255441019,-0.173641515864913,
2.4));
#10713=CARTESIAN_POINT('Ctrl Pts',(0.0286575889694474,-0.173002476522168,
2.4));
#10714=CARTESIAN_POINT('Ctrl Pts',(0.0309968484005323,-0.172308959609585,
2.4));
#10715=CARTESIAN_POINT('Ctrl Pts',(0.0349907200356912,-0.171124902172917,
2.4));
#10716=CARTESIAN_POINT('Ctrl Pts',(0.0389417632399139,-0.169782062987551,
2.4));
#10717=CARTESIAN_POINT('Ctrl Pts',(0.0428430867479635,-0.168285488070655,
2.4));
#10718=CARTESIAN_POINT('Ctrl Pts',(0.0460795423288881,-0.167043961129333,
2.4));
#10719=CARTESIAN_POINT('Ctrl Pts',(0.0492804988882749,-0.1656968372236,
2.4));
#10720=CARTESIAN_POINT('Ctrl Pts',(0.0524310205930229,-0.164252769154906,
2.4));
#10721=CARTESIAN_POINT('Ctrl Pts',(0.0632193618964415,-0.159307842361683,
2.4));
#10722=CARTESIAN_POINT('Ctrl Pts',(0.0734566084017215,-0.153215648615148,
2.4));
#10723=CARTESIAN_POINT('Ctrl Pts',(0.0829954583811563,-0.146117480833417,
2.4));
#10724=CARTESIAN_POINT('Ctrl Pts',(0.0871250594161281,-0.143044510707979,
2.4));
#10725=CARTESIAN_POINT('Ctrl Pts',(0.0911232569109863,-0.139782483459033,
2.4));
#10726=CARTESIAN_POINT('Ctrl Pts',(0.0949753370068491,-0.136341074649165,
2.4));
#10727=CARTESIAN_POINT('Ctrl Pts',(0.0986768888660373,-0.133034146220529,
2.4));
#10728=CARTESIAN_POINT('Ctrl Pts',(0.102245690547589,-0.129558617700049,
2.4));
#10729=CARTESIAN_POINT('Ctrl Pts',(0.105650031744245,-0.125942409265612,
2.4));
#10730=CARTESIAN_POINT('Ctrl Pts',(0.111001095053008,-0.120258325575831,
2.4));
#10731=CARTESIAN_POINT('Ctrl Pts',(0.115956461643762,-0.114218962093958,
2.4));
#10732=CARTESIAN_POINT('Ctrl Pts',(0.120465674061468,-0.107861150525121,
2.4));
#10733=CARTESIAN_POINT('Ctrl Pts',(0.122806690655693,-0.10456040950721,
2.4));
#10734=CARTESIAN_POINT('Ctrl Pts',(0.125027588538421,-0.101173242254719,
2.4));
#10735=CARTESIAN_POINT('Ctrl Pts',(0.127119040336103,-0.0977061228092429,
2.4));
#10736=CARTESIAN_POINT('Ctrl Pts',(0.132655068544743,-0.0885287317385256,
2.4));
#10737=CARTESIAN_POINT('Ctrl Pts',(0.13725573814533,-0.0788453760087664,
2.4));
#10738=CARTESIAN_POINT('Ctrl Pts',(0.140775482942457,-0.0687522252708787,
2.4));
#10739=CARTESIAN_POINT('Ctrl Pts',(0.141790390598368,-0.0658418961002798,
2.4));
#10740=CARTESIAN_POINT('Ctrl Pts',(0.142715102613091,-0.0628974577303924,
2.4));
#10741=CARTESIAN_POINT('Ctrl Pts',(0.143545299885864,-0.0599211930845618,
2.4));
#10742=CARTESIAN_POINT('Ctrl Pts',(-0.195373070919361,0.000178101583232409,
2.39241303078758));
#10743=CARTESIAN_POINT('Ctrl Pts',(-0.194995765056209,-0.044191626196564,
2.39494202052505));
#10744=CARTESIAN_POINT('Ctrl Pts',(-0.17967283890898,-0.0888121436870032,
2.39747101026252));
#10745=CARTESIAN_POINT('Ctrl Pts',(-0.152022961461301,-0.123275749177746,
2.4));
#10746=CARTESIAN_POINT('',(-0.0903606778650279,-0.126612599672279,0.));
#10747=CARTESIAN_POINT('Ctrl Pts',(-0.0905547187627355,-0.126790994435269,
1.73472347597681E-18));
#10748=CARTESIAN_POINT('Ctrl Pts',(-0.0937786982673177,-0.125067385071004,
2.04138089632303E-18));
#10749=CARTESIAN_POINT('Ctrl Pts',(-0.0969317870940273,-0.123225562125392,
4.55088741215883E-19));
#10750=CARTESIAN_POINT('Ctrl Pts',(-0.100006715605072,-0.121266986978485,
-4.55364912443912E-18));
#10751=CARTESIAN_POINT('Ctrl Pts',(-0.107443591426499,-0.116530070298256,
-1.67607735186196E-17));
#10752=CARTESIAN_POINT('Ctrl Pts',(-0.114423960357848,-0.111111926712958,
-1.67652824684633E-17));
#10753=CARTESIAN_POINT('Ctrl Pts',(-0.120920626723682,-0.105114084706666,
1.90819582357449E-17));
#10754=CARTESIAN_POINT('Ctrl Pts',(-0.123989218118145,-0.102281104632047,
3.60138011450046E-17));
#10755=CARTESIAN_POINT('Ctrl Pts',(-0.126949571175365,-0.0993181071661729,
-2.80225227290868E-17));
#10756=CARTESIAN_POINT('Ctrl Pts',(-0.129788621846087,-0.0962459886237453,
-2.73218947466347E-17));
#10757=CARTESIAN_POINT('Ctrl Pts',(-0.135122303451826,-0.0904744459283742,
-2.60056355403416E-17));
#10758=CARTESIAN_POINT('Ctrl Pts',(-0.140037740247948,-0.0843101296795999,
-2.18057762441945E-17));
#10759=CARTESIAN_POINT('Ctrl Pts',(-0.144515198029218,-0.0778188929962127,
-1.12757025938492E-17));
#10760=CARTESIAN_POINT('Ctrl Pts',(-0.14680932318637,-0.0744929633942239,
-5.88038497210284E-18));
#10761=CARTESIAN_POINT('Ctrl Pts',(-0.148989224672256,-0.0710795596597342,
1.31303430263246E-17));
#10762=CARTESIAN_POINT('Ctrl Pts',(-0.151048822309793,-0.0675910768160332,
1.12757025938492E-17));
#10763=CARTESIAN_POINT('Ctrl Pts',(-0.156978439475454,-0.0575476744664053,
5.93616076096574E-18));
#10764=CARTESIAN_POINT('Ctrl Pts',(-0.161879094027928,-0.0469447472885605,
1.60901821933146E-17));
#10765=CARTESIAN_POINT('Ctrl Pts',(-0.165691488986893,-0.0359818104818786,
3.46944695195361E-18));
#10766=CARTESIAN_POINT('Ctrl Pts',(-0.168615156166144,-0.0275745025101442,
-6.20920119451492E-18));
#10767=CARTESIAN_POINT('Ctrl Pts',(-0.170898487612157,-0.0189541362718905,
7.18953415028294E-18));
#10768=CARTESIAN_POINT('Ctrl Pts',(-0.172499257712041,-0.0101976684652424,
5.20417042793042E-18));
#10769=CARTESIAN_POINT('Ctrl Pts',(-0.173128740734504,-0.00675429591510353,
4.42345072512973E-18));
#10770=CARTESIAN_POINT('Ctrl Pts',(-0.173652109787855,-0.00329034195238573,
-8.72241236130908E-18));
#10771=CARTESIAN_POINT('Ctrl Pts',(-0.174065393356307,0.000176078536121731,
-8.67361737988404E-18));
#10772=CARTESIAN_POINT('Ctrl Pts',(-0.174874448648527,0.0069620387227214,
-8.57809498081156E-18));
#10773=CARTESIAN_POINT('Ctrl Pts',(-0.17526451573988,0.0137702403350294,
-1.47546100136584E-17));
#10774=CARTESIAN_POINT('Ctrl Pts',(-0.17522174425039,0.020564792502022,
-1.04083408558608E-17));
#10775=CARTESIAN_POINT('Ctrl Pts',(-0.175173289109206,0.028262232747164,
-7.43567664424826E-18));
#10776=CARTESIAN_POINT('Ctrl Pts',(-0.174569669212428,0.0359422811365838,
-3.66078693759541E-17));
#10777=CARTESIAN_POINT('Ctrl Pts',(-0.173446373975917,0.0435656717636881,
-4.5102810375397E-17));
#10778=CARTESIAN_POINT('Ctrl Pts',(-0.17276034872808,0.0482214721929289,
-5.02908889989642E-17));
#10779=CARTESIAN_POINT('Ctrl Pts',(-0.171880287491841,0.0528561871195019,
-2.94043840421531E-18));
#10780=CARTESIAN_POINT('Ctrl Pts',(-0.170812464892208,0.0574609818532008,
-6.93889390390723E-18));
#10781=CARTESIAN_POINT('Ctrl Pts',(-0.170006933705219,0.0609346915957652,
-9.95520073792165E-18));
#10782=CARTESIAN_POINT('Ctrl Pts',(-0.169094445764795,0.0643905438353253,
-1.22076013790627E-17));
#10783=CARTESIAN_POINT('Ctrl Pts',(-0.168081936099544,0.0678120165229409,
-1.38777878078145E-17));
#10784=CARTESIAN_POINT('Ctrl Pts',(-0.164824625672852,0.0788191200030298,
-1.92508877945114E-17));
#10785=CARTESIAN_POINT('Ctrl Pts',(-0.160527857603151,0.0895048987030934,
-1.40762953787734E-17));
#10786=CARTESIAN_POINT('Ctrl Pts',(-0.15530139184747,0.0997465174632775,
-6.93889390390723E-18));
#10787=CARTESIAN_POINT('Ctrl Pts',(-0.152082958509342,0.106053258728798,
-2.54371522520859E-18));
#10788=CARTESIAN_POINT('Ctrl Pts',(-0.148511119845249,0.112191703210516,
-2.81380830112988E-17));
#10789=CARTESIAN_POINT('Ctrl Pts',(-0.144604138031713,0.118132165785462,
-2.42861286636753E-17));
#10790=CARTESIAN_POINT('Ctrl Pts',(-0.141699683152471,0.122548312656426,
-2.14225812673671E-17));
#10791=CARTESIAN_POINT('Ctrl Pts',(-0.138605937056638,0.126859392699012,
-1.20788926485952E-17));
#10792=CARTESIAN_POINT('Ctrl Pts',(-0.135350387038284,0.131026597701989,
-1.38777878078145E-17));
#10793=CARTESIAN_POINT('Ctrl Pts',(-0.127454964434828,0.141132983531803,
-1.82405029930444E-17));
#10794=CARTESIAN_POINT('Ctrl Pts',(-0.118596896875794,0.150421116028237,
3.19066915871575E-18));
#10795=CARTESIAN_POINT('Ctrl Pts',(-0.108893943796901,0.158727847366355,
1.73472347597681E-17));
#10796=CARTESIAN_POINT('Ctrl Pts',(-0.101760675780719,0.164834662527825,
2.77546412266345E-17));
#10797=CARTESIAN_POINT('Ctrl Pts',(-0.0941695959020444,0.170411093356264,
-5.23705385272153E-18));
#10798=CARTESIAN_POINT('Ctrl Pts',(-0.0861525859670525,0.175382131162755,
-6.93889390390723E-18));
#10799=CARTESIAN_POINT('Ctrl Pts',(-0.090554718762734,-0.12679099443527,
1.38750773023832E-16));
#10800=CARTESIAN_POINT('Ctrl Pts',(-0.0514132965269827,-0.154438798808553,
0.00344557680604053));
#10801=CARTESIAN_POINT('Ctrl Pts',(0.0585934425206843,-0.172181219813116,
0.0105960579060063));
#10802=CARTESIAN_POINT('Ctrl Pts',(0.177419525591119,-0.0482168938798953,
0.0214514432998975));
#10803=CARTESIAN_POINT('Ctrl Pts',(0.13670630608002,0.122966787890628,0.0325661561816737));
#10804=CARTESIAN_POINT('Ctrl Pts',(-0.0291762440449378,0.181518694867924,
0.0436808690634499));
#10805=CARTESIAN_POINT('Ctrl Pts',(-0.141190839714012,0.0949193830602739,
0.0526273578563488));
#10806=CARTESIAN_POINT('Ctrl Pts',(-0.155411338149369,0.021598754870737,
0.0578689423553222));
#10807=CARTESIAN_POINT('Ctrl Pts',(-0.155324515707295,7.08434145518418E-5,
0.0594056225603703));
#10808=CARTESIAN_POINT('Origin',(0.,0.,-0.129405622560373));
#10809=CARTESIAN_POINT('',(0.090360677865021,-0.126612599672283,0.));
#10810=CARTESIAN_POINT('Origin',(0.,0.,0.));
#10811=CARTESIAN_POINT('Ctrl Pts',(0.0903606778650135,-0.126612599672289,
0.));
#10812=CARTESIAN_POINT('Ctrl Pts',(0.132465879166514,-0.0965630268723143,
0.0037049042939254));
#10813=CARTESIAN_POINT('Ctrl Pts',(0.183615222457176,0.00832016090824247,
0.0111147128817762));
#10814=CARTESIAN_POINT('Ctrl Pts',(0.0924018852348323,0.159092396164803,
0.0222294257635523));
#10815=CARTESIAN_POINT('Ctrl Pts',(-0.0834773491744035,0.163753054047276,
0.0333441386453285));
#10816=CARTESIAN_POINT('Ctrl Pts',(-0.153142789995597,0.0621407336789083,
0.0411324558706874));
#10817=CARTESIAN_POINT('Ctrl Pts',(-0.155773969573712,0.00536683624356025,
0.0452158688021209));
#10818=CARTESIAN_POINT('Ctrl Pts',(-0.155737693224454,0.000100603112028588,
0.045594377439629));
#10819=CARTESIAN_POINT('Ctrl Pts',(0.113509973994375,-0.15904919303095,
-0.0230074082272066));
#10820=CARTESIAN_POINT('Ctrl Pts',(0.166402010859132,-0.121301288658623,
-0.0193025039332812));
#10821=CARTESIAN_POINT('Ctrl Pts',(0.230655187837557,0.0104516839696087,
-0.0118926953454304));
#10822=CARTESIAN_POINT('Ctrl Pts',(0.116074113628315,0.199849914565114,
-0.000777982463654263));
#10823=CARTESIAN_POINT('Ctrl Pts',(-0.104863221013695,0.2057045757688,0.010336730418122));
#10824=CARTESIAN_POINT('Ctrl Pts',(-0.229752900032261,0.0235435225184469,
0.0214514432998981));
#10825=CARTESIAN_POINT('Ctrl Pts',(-0.144341709283358,-0.180324797442481,
0.0325661561816743));
#10826=CARTESIAN_POINT('Ctrl Pts',(0.0732211700541786,-0.219033718527301,
0.0436808690634505));
#10827=CARTESIAN_POINT('Ctrl Pts',(0.223746334253748,-0.0572705996896121,
0.0547955819452267));
#10828=CARTESIAN_POINT('Ctrl Pts',(0.169446625860147,0.156943281339981,
0.0659102948270027));
#10829=CARTESIAN_POINT('Ctrl Pts',(-0.0399751411601898,0.227471578691002,
0.0770250077087791));
#10830=CARTESIAN_POINT('Ctrl Pts',(-0.212800571019475,0.0897670413771846,
0.088139720590555));
#10831=CARTESIAN_POINT('Ctrl Pts',(-0.190818134346944,-0.13011804196319,
0.0992544334723316));
#10832=CARTESIAN_POINT('Ctrl Pts',(0.00584918801334432,-0.230884768458966,
0.110369146354107));
#10833=CARTESIAN_POINT('Ctrl Pts',(0.197161712231628,-0.120288773936248,
0.121483859235884));
#10834=CARTESIAN_POINT('Ctrl Pts',(0.207982494406915,0.100426132144772,
0.13259857211766));
#10835=CARTESIAN_POINT('Ctrl Pts',(0.0284055178284121,0.229205619323633,
0.143713284999436));
#10836=CARTESIAN_POINT('Ctrl Pts',(-0.177175286844647,0.148158796784502,
0.154827997881212));
#10837=CARTESIAN_POINT('Ctrl Pts',(-0.220560866541884,-0.068520165527927,
0.165942710762988));
#10838=CARTESIAN_POINT('Ctrl Pts',(-0.0620338447715747,-0.222472259699958,
0.177057423644765));
#10839=CARTESIAN_POINT('Ctrl Pts',(0.153282099103901,-0.172761991393912,
0.188172136526541));
#10840=CARTESIAN_POINT('Ctrl Pts',(0.228275842850265,0.0351033693558483,
0.199286849408317));
#10841=CARTESIAN_POINT('Ctrl Pts',(0.0942943101399089,0.210833321528243,
0.210401562290093));
#10842=CARTESIAN_POINT('Ctrl Pts',(-0.126009012428097,0.193555768902392,
0.221516275171869));
#10843=CARTESIAN_POINT('Ctrl Pts',(-0.230957299139034,-0.000912545418766224,
0.232630988053646));
#10844=CARTESIAN_POINT('Ctrl Pts',(-0.124475569182979,-0.194545468655793,
0.243745700935422));
#10845=CARTESIAN_POINT('Ctrl Pts',(0.0959574051494835,-0.210081610730679,
0.254860413817198));
#10846=CARTESIAN_POINT('Ctrl Pts',(0.228546107728123,-0.0332983992076444,
0.265975126698974));
#10847=CARTESIAN_POINT('Ctrl Pts',(0.151912120568595,0.173967854400789,
0.277089839580751));
#10848=CARTESIAN_POINT('Ctrl Pts',(-0.0637899206477135,0.221975117467028,
0.288204552462526));
#10849=CARTESIAN_POINT('Ctrl Pts',(-0.221095435638538,0.0667751082861117,
0.299319265344303));
#10850=CARTESIAN_POINT('Ctrl Pts',(-0.175998983737975,-0.149554219162863,
0.310433978226078));
#10851=CARTESIAN_POINT('Ctrl Pts',(0.0302158574941517,-0.22897403499859,
0.321548691107855));
#10852=CARTESIAN_POINT('Ctrl Pts',(0.208769571438822,-0.0987794148000734,
0.332663403989631));
#10853=CARTESIAN_POINT('Ctrl Pts',(0.196205039257046,0.121842887839669,
0.343778116871407));
#10854=CARTESIAN_POINT('Ctrl Pts',(0.0040244704784676,0.230924035961029,
0.354892829753183));
#10855=CARTESIAN_POINT('Ctrl Pts',(-0.191840302536165,0.12860561834497,
0.366007542634959));
#10856=CARTESIAN_POINT('Ctrl Pts',(-0.212084740152647,-0.0914449000297386,
0.377122255516736));
#10857=CARTESIAN_POINT('Ctrl Pts',(-0.038176058189903,-0.227782122494658,
0.388236968398511));
#10858=CARTESIAN_POINT('Ctrl Pts',(0.170680922200525,-0.155596046041835,
0.399351681280289));
#10859=CARTESIAN_POINT('Ctrl Pts',(0.223287936308385,0.0590305365571002,
0.410466394162064));
#10860=CARTESIAN_POINT('Ctrl Pts',(0.071485857298635,0.21961757432719,0.421581107043841));
#10861=CARTESIAN_POINT('Ctrl Pts',(-0.145757998381792,0.179155554350991,
0.432695819925616));
#10862=CARTESIAN_POINT('Ctrl Pts',(-0.2295675953358,-0.0253145396722107,
0.443810532807393));
#10863=CARTESIAN_POINT('Ctrl Pts',(-0.103219381045708,-0.206610421139929,
0.454925245689169));
#10864=CARTESIAN_POINT('Ctrl Pts',(0.117621085806451,-0.198764652090831,
0.466039958570945));
#10865=CARTESIAN_POINT('Ctrl Pts',(0.230785249680916,-0.00895964713562851,
0.477154671452722));
#10866=CARTESIAN_POINT('Ctrl Pts',(0.132676899813103,0.189047472881977,
0.488269384334497));
#10867=CARTESIAN_POINT('Ctrl Pts',(-0.0868906082019593,0.213990955307395,
0.499384097216274));
#10868=CARTESIAN_POINT('Ctrl Pts',(-0.226914049857475,0.0430362721940153,
0.51049881009805));
#10869=CARTESIAN_POINT('Ctrl Pts',(-0.159208870281294,-0.167315995561787,
0.521613522979826));
#10870=CARTESIAN_POINT('Ctrl Pts',(0.0542441778475903,-0.224498721414436,
0.532728235861603));
#10871=CARTESIAN_POINT('Ctrl Pts',(0.218039356482698,-0.0761639401008682,
0.543842948743378));
#10872=CARTESIAN_POINT('Ctrl Pts',(0.182230257970378,0.14189517196553,0.554957661625155));
#10873=CARTESIAN_POINT('Ctrl Pts',(-0.0204016541079569,0.230056252374799,
0.566072374506931));
#10874=CARTESIAN_POINT('Ctrl Pts',(-0.204356858061106,0.107612180121354,
0.577187087388706));
#10875=CARTESIAN_POINT('Ctrl Pts',(-0.201233437350254,-0.113345535594831,
0.588301800270484));
#10876=CARTESIAN_POINT('Ctrl Pts',(-0.0138907295889131,-0.2305410036817,
0.599416513152259));
#10877=CARTESIAN_POINT('Ctrl Pts',(0.186168256019567,-0.136687553192347,
0.610531226034036));
#10878=CARTESIAN_POINT('Ctrl Pts',(0.21579938507027,0.0822966108073177,
0.621645938915812));
#10879=CARTESIAN_POINT('Ctrl Pts',(0.0478768203261135,0.225942286486038,
0.632760651797588));
#10880=CARTESIAN_POINT('Ctrl Pts',(-0.163874612139314,0.162748942372192,
0.643875364679364));
#10881=CARTESIAN_POINT('Ctrl Pts',(-0.225606919495652,-0.0494330316970348,
0.654990077561141));
#10882=CARTESIAN_POINT('Ctrl Pts',(-0.0808072189988052,-0.216361503287338,
0.666104790442916));
#10883=CARTESIAN_POINT('Ctrl Pts',(0.137967505075176,-0.185221689578757,
0.677219503324693));
#10884=CARTESIAN_POINT('Ctrl Pts',(0.230439782817408,0.0154794457957462,
0.688334216206469));
#10885=CARTESIAN_POINT('Ctrl Pts',(0.111955804692462,0.20200991199132,0.699448929088245));
#10886=CARTESIAN_POINT('Ctrl Pts',(-0.109018190962282,0.203610266898281,
0.710563641970021));
#10887=CARTESIAN_POINT('Ctrl Pts',(-0.230191409573946,0.0188154645288922,
0.721678354851798));
#10888=CARTESIAN_POINT('Ctrl Pts',(-0.140635745773037,-0.183203967637002,
0.732793067733573));
#10889=CARTESIAN_POINT('Ctrl Pts',(0.0776650071207401,-0.217509203060499,
0.74390778061535));
#10890=CARTESIAN_POINT('Ctrl Pts',(0.224867276437698,-0.0526954906473946,
0.755022493497126));
#10891=CARTESIAN_POINT('Ctrl Pts',(0.166214644641793,0.160358344509041,
0.766137206378902));
#10892=CARTESIAN_POINT('Ctrl Pts',(-0.044599296608695,0.226612024149398,
0.777251919260677));
#10893=CARTESIAN_POINT('Ctrl Pts',(-0.214584781453568,0.08541357219788,
0.788366632142455));
#10894=CARTESIAN_POINT('Ctrl Pts',(-0.188128482210358,-0.133976792498943,
0.799481345024231));
#10895=CARTESIAN_POINT('Ctrl Pts',(0.0105501639898399,-0.230718011405407,
0.810596057906007));
#10896=CARTESIAN_POINT('Ctrl Pts',(0.19957065539198,-0.116248269894625,
0.821710770787783));
#10897=CARTESIAN_POINT('Ctrl Pts',(0.205894054617937,0.104641029333927,
0.832825483669559));
#10898=CARTESIAN_POINT('Ctrl Pts',(0.0237316015467294,0.229736627108315,
0.843940196551335));
#10899=CARTESIAN_POINT('Ctrl Pts',(-0.180155962296678,0.144519673387521,
0.855054909433111));
#10900=CARTESIAN_POINT('Ctrl Pts',(-0.219119627958972,-0.0729979136016889,
0.866169622314888));
#10901=CARTESIAN_POINT('Ctrl Pts',(-0.0574900812163527,-0.223689510949474,
0.877284335196663));
#10902=CARTESIAN_POINT('Ctrl Pts',(0.15676879946602,-0.16960439340141,0.88839904807844));
#10903=CARTESIAN_POINT('Ctrl Pts',(0.227513576082652,0.0397451814080778,
0.899513760960216));
#10904=CARTESIAN_POINT('Ctrl Pts',(0.0899808947771051,0.212710002872901,
0.910628473841993));
#10905=CARTESIAN_POINT('Ctrl Pts',(-0.129924857834439,0.190949307576065,
0.921743186723768));
#10906=CARTESIAN_POINT('Ctrl Pts',(-0.230890810999347,-0.00561606117680894,
0.932857899605545));
#10907=CARTESIAN_POINT('Ctrl Pts',(-0.120487614241242,-0.197040202906745,
0.943972612487321));
#10908=CARTESIAN_POINT('Ctrl Pts',(0.100216050899275,-0.208083756908682,
0.955087325369097));
#10909=CARTESIAN_POINT('Ctrl Pts',(0.229176864102385,-0.0286368941625087,
0.966202038250873));
#10910=CARTESIAN_POINT('Ctrl Pts',(0.148337561234701,0.177025632816322,
0.97731675113265));
#10911=CARTESIAN_POINT('Ctrl Pts',(-0.0682974629270641,0.220629923865291,
0.988431464014425));
#10912=CARTESIAN_POINT('Ctrl Pts',(-0.22240952821355,0.0622584010949852,
0.999546176896202));
#10913=CARTESIAN_POINT('Ctrl Pts',(-0.17291663967011,-0.153107617290177,
1.01066088977798));
#10914=CARTESIAN_POINT('Ctrl Pts',(0.0348729042335921,-0.228311163321885,
1.02177560265975));
#10915=CARTESIAN_POINT('Ctrl Pts',(0.210738024244903,-0.0945070996509389,
1.03289031554153));
#10916=CARTESIAN_POINT('Ctrl Pts',(0.193682876670397,0.125813552655338,
1.04400502842331));
#10917=CARTESIAN_POINT('Ctrl Pts',(-0.000679392046237043,0.230958102636658,
1.05511974130508));
#10918=CARTESIAN_POINT('Ctrl Pts',(-0.194419710852192,0.124671900519835,
1.06623445418686));
#10919=CARTESIAN_POINT('Ctrl Pts',(-0.210178373163287,-0.095745277698235,
1.07734916706864));
#10920=CARTESIAN_POINT('Ctrl Pts',(-0.0335291008517639,-0.22851237634568,
1.08846387995041));
#10921=CARTESIAN_POINT('Ctrl Pts',(0.173814409632538,-0.152087664691026,
1.09957859283219));
#10922=CARTESIAN_POINT('Ctrl Pts',(0.222039400634039,0.0635658030166745,
1.11069330571397));
#10923=CARTESIAN_POINT('Ctrl Pts',(0.0669982713499448,0.221027913131344,
1.12180801859574));
#10924=CARTESIAN_POINT('Ctrl Pts',(-0.149376470996772,0.176149869882519,
1.13292273147752));
#10925=CARTESIAN_POINT('Ctrl Pts',(-0.229004421401316,-0.0299846915229451,
1.14403744435929));
#10926=CARTESIAN_POINT('Ctrl Pts',(-0.0989901185230116,-0.208669746685709,
1.15515215724107));
#10927=CARTESIAN_POINT('Ctrl Pts',(0.121644755665281,-0.196327940360541,
1.16626687012285));
#10928=CARTESIAN_POINT('Ctrl Pts',(0.230919855567728,-0.00425758753959744,
1.17738158300462));
#10929=CARTESIAN_POINT('Ctrl Pts',(0.12879921667729,0.191710376689407,1.1884962958864));
#10930=CARTESIAN_POINT('Ctrl Pts',(-0.0912307526970952,0.212176946225077,
1.19961100876817));
#10931=CARTESIAN_POINT('Ctrl Pts',(-0.227743467482791,0.0384059860697885,
1.21072572164995));
#10932=CARTESIAN_POINT('Ctrl Pts',(-0.155768270107734,-0.170523760147147,
1.22184043453172));
#10933=CARTESIAN_POINT('Ctrl Pts',(0.0588050960517139,-0.22334741419015,
1.2329551474135));
#10934=CARTESIAN_POINT('Ctrl Pts',(0.219545297046235,-0.071707526048235,
1.24406986029528));
#10935=CARTESIAN_POINT('Ctrl Pts',(0.179302606580475,0.145577065571899,
1.25518457317705));
#10936=CARTESIAN_POINT('Ctrl Pts',(-0.0250827769957638,0.229593033529458,
1.26629928605883));
#10937=CARTESIAN_POINT('Ctrl Pts',(-0.206506115316257,0.103427902831233,
1.27741399894061));
#10938=CARTESIAN_POINT('Ctrl Pts',(-0.198883289957136,-0.1174203718394,
1.28852871182238));
#10939=CARTESIAN_POINT('Ctrl Pts',(-0.00919262157653787,-0.23077608726995,
1.29964342470416));
#10940=CARTESIAN_POINT('Ctrl Pts',(0.188913438476804,-0.132867676693576,
1.31075813758593));
#10941=CARTESIAN_POINT('Ctrl Pts',(0.214078562825313,0.0866745388549966,
1.32187285046771));
#10942=CARTESIAN_POINT('Ctrl Pts',(0.0432653212731772,0.226870488874615,
1.33298756334948));
#10943=CARTESIAN_POINT('Ctrl Pts',(-0.167155188056641,0.159377695593915,
1.34410227623126));
#10944=CARTESIAN_POINT('Ctrl Pts',(-0.224553366823233,-0.0540175174867204,
1.35521698911304));
#10945=CARTESIAN_POINT('Ctrl Pts',(-0.0763840132469668,-0.217962357455055,
1.36633170199482));
#10946=CARTESIAN_POINT('Ctrl Pts',(0.141711137193365,-0.182373409088171,
1.37744641487659));
#10947=CARTESIAN_POINT('Ctrl Pts',(0.230076730733878,0.020169400632847,
1.38856112775837));
#10948=CARTESIAN_POINT('Ctrl Pts',(0.107818424683935,0.204248118830388,
1.39967584064014));
#10949=CARTESIAN_POINT('Ctrl Pts',(-0.113142331553799,0.201347757766626,
1.41079055352192));
#10950=CARTESIAN_POINT('Ctrl Pts',(-0.230526863439747,0.0141234549494752,
1.4219052664037));
#10951=CARTESIAN_POINT('Ctrl Pts',(-0.136875421443584,-0.186030174304383,
1.43301997928547));
#10952=CARTESIAN_POINT('Ctrl Pts',(0.0820787181812268,-0.215882354000517,
1.44413469216725));
#10953=CARTESIAN_POINT('Ctrl Pts',(0.225893839437804,-0.048104885938183,
1.45524940504902));
#10954=CARTESIAN_POINT('Ctrl Pts',(0.162914291785062,0.163710232665064,
1.4663641179308));
#10955=CARTESIAN_POINT('Ctrl Pts',(-0.0492052550555011,0.225656707460693,
1.47747883081258));
#10956=CARTESIAN_POINT('Ctrl Pts',(-0.21627981769851,0.0810255959766872,
1.48859354369435));
#10957=CARTESIAN_POINT('Ctrl Pts',(-0.185360874170467,-0.137780452437339,
1.49970825657613));
#10958=CARTESIAN_POINT('Ctrl Pts',(0.0152468076526161,-0.230455291984111,
1.51082296945791));
#10959=CARTESIAN_POINT('Ctrl Pts',(0.201896789043082,-0.112159677786499,
1.52193768233968));
#10960=CARTESIAN_POINT('Ctrl Pts',(0.203720217624815,0.108812589703471,
1.53305239522146));
#10961=CARTESIAN_POINT('Ctrl Pts',(0.0190478344628315,0.230172297962536,
1.54416710810323));
#10962=CARTESIAN_POINT('Ctrl Pts',(-0.18306190170968,0.140820619546688,
1.55528182098501));
#10963=CARTESIAN_POINT('Ctrl Pts',(-0.217587495489559,-0.0774453907838218,
1.56639653386679));
#10964=CARTESIAN_POINT('Ctrl Pts',(-0.0529224685754187,-0.224813965462472,
1.57751124674856));
#10965=CARTESIAN_POINT('Ctrl Pts',(0.160190468180596,-0.166376442596779,
1.58862595963034));
#10966=CARTESIAN_POINT('Ctrl Pts',(0.226656931919555,0.0443705077714034,
1.59974067251212));
#10967=CARTESIAN_POINT('Ctrl Pts',(0.0856301532179132,0.214498446630633,
1.61085538539389));
#10968=CARTESIAN_POINT('Ctrl Pts',(-0.133786807471087,0.188263636674139,
1.62197009827567));
#10969=CARTESIAN_POINT('Ctrl Pts',(-0.230728544292657,-0.0103172474851095,
1.63308481115744));
#10970=CARTESIAN_POINT('Ctrl Pts',(-0.116449678358188,-0.199453200418927,
1.64419952403922));
#10971=CARTESIAN_POINT('Ctrl Pts',(0.104433124808968,-0.205999585411506,
1.655314236921));
#10972=CARTESIAN_POINT('Ctrl Pts',(0.229712552860698,-0.0239635098701923,
1.66642894980277));
#10973=CARTESIAN_POINT('Ctrl Pts',(0.144701468203596,0.180009977075721,
1.67754366268455));
#10974=CARTESIAN_POINT('Ctrl Pts',(-0.0727766739099085,0.219193208110308,
1.68865837556633));
#10975=CARTESIAN_POINT('Ctrl Pts',(-0.22363136040826,0.0577158677404108,
1.6997730884481));
#10976=CARTESIAN_POINT('Ctrl Pts',(-0.169762565963256,-0.156597502996213,
1.71088780132988));
#10977=CARTESIAN_POINT('Ctrl Pts',(0.039515484922465,-0.227553583136852,
1.72200251421165));
#10978=CARTESIAN_POINT('Ctrl Pts',(0.212619058267456,-0.0901955808703403,
1.73311722709343));
#10979=CARTESIAN_POINT('Ctrl Pts',(0.191080370151679,0.129732027232196,
1.7442319399752));
#10980=CARTESIAN_POINT('Ctrl Pts',(-0.00538297274409746,0.230896362794034,
1.75534665285698));
#10981=CARTESIAN_POINT('Ctrl Pts',(-0.19691846958115,0.120686466038639,
1.76646136573876));
#10982=CARTESIAN_POINT('Ctrl Pts',(-0.208184819545892,-0.100005938112305,
1.77757607862054));
#10983=CARTESIAN_POINT('Ctrl Pts',(-0.0288682349025721,-0.229147838219538,
1.78869079150231));
#10984=CARTESIAN_POINT('Ctrl Pts',(0.176875795011193,-0.148516194020166,
1.79980550438409));
#10985=CARTESIAN_POINT('Ctrl Pts',(0.220698758115687,0.0680747009781974,
1.81092021726586));
#10986=CARTESIAN_POINT('Ctrl Pts',(0.0624828930395807,0.222346564678841,
1.82203493014764));
#10987=CARTESIAN_POINT('Ctrl Pts',(-0.152932978954706,0.173071114560221,
1.83314964302941));
#10988=CARTESIAN_POINT('Ctrl Pts',(-0.22834625137849,-0.0346424050618476,
1.84426435591119));
#10989=CARTESIAN_POINT('Ctrl Pts',(-0.094719792714343,-0.210642511415027,
1.85537906879297));
#10990=CARTESIAN_POINT('Ctrl Pts',(0.125617964594648,-0.193809787467443,
1.86649378167474));
#10991=CARTESIAN_POINT('Ctrl Pts',(0.230958670801831,0.000446238197717259,
1.87760849455652));
#10992=CARTESIAN_POINT('Ctrl Pts',(0.124868104783677,0.194293754801359,
1.88872320743829));
#10993=CARTESIAN_POINT('Ctrl Pts',(-0.095533052662467,0.210274921462518,
1.89983792032007));
#10994=CARTESIAN_POINT('Ctrl Pts',(-0.228478412091282,0.0337597682948806,
1.91095263320185));
#10995=CARTESIAN_POINT('Ctrl Pts',(-0.152263053817779,-0.17366078771318,
1.92206734608362));
#10996=CARTESIAN_POINT('Ctrl Pts',(0.0633416206041145,-0.222103457528968,
1.9331820589654));
#10997=CARTESIAN_POINT('Ctrl Pts',(0.220960165374983,-0.0672213661311443,
1.94429677184717));
#10998=CARTESIAN_POINT('Ctrl Pts',(0.176300576511988,0.149198570598448,
1.95541148472895));
#10999=CARTESIAN_POINT('Ctrl Pts',(-0.0297534949940769,0.229034574426469,
1.96652619761073));
#11000=CARTESIAN_POINT('Ctrl Pts',(-0.208569709276974,0.0992007213642766,
1.97764091049251));
#11001=CARTESIAN_POINT('Ctrl Pts',(-0.196450641385828,-0.121446499522165,
1.98875562337428));
#11002=CARTESIAN_POINT('Ctrl Pts',(-0.00449070026179651,-0.230915439843731,
1.99987033625606));
#11003=CARTESIAN_POINT('Ctrl Pts',(0.191580255470184,-0.128992683750042,
2.01098504913783));
#11004=CARTESIAN_POINT('Ctrl Pts',(0.212268936067735,0.091016512391074,
2.02209976201961));
#11005=CARTESIAN_POINT('Ctrl Pts',(0.0386358748097637,0.227704580376973,
2.03321447490139));
#11006=CARTESIAN_POINT('Ctrl Pts',(-0.170366424312123,0.155940335430241,
2.04432918778316));
#11007=CARTESIAN_POINT('Ctrl Pts',(-0.223406664459236,-0.05857959561862,
2.05544390066494));
#11008=CARTESIAN_POINT('Ctrl Pts',(-0.0719291217184943,-0.219472796024974,
2.06655861354672));
#11009=CARTESIAN_POINT('Ctrl Pts',(0.145395984400223,-0.179449476084793,
2.07767332642849));
#11010=CARTESIAN_POINT('Ctrl Pts',(0.229618237751902,0.0248509887620852,
2.08878803931027));
#11011=CARTESIAN_POINT('Ctrl Pts',(0.103636319198972,0.20640159903293,2.09990275219204));
#11012=CARTESIAN_POINT('Ctrl Pts',(-0.117219538181985,0.199001725158021,
2.11101746507382));
#11013=CARTESIAN_POINT('Ctrl Pts',(-0.230766689726102,0.00942558661705901,
2.1221321779556));
#11014=CARTESIAN_POINT('Ctrl Pts',(-0.133058318070465,-0.188779211488415,
2.13324689083737));
#11015=CARTESIAN_POINT('Ctrl Pts',(0.0864583809916643,-0.214165952291765,
2.14436160371915));
#11016=CARTESIAN_POINT('Ctrl Pts',(0.22682669704182,-0.043494326039136,
2.15547631660092));
#11017=CARTESIAN_POINT('Ctrl Pts',(0.159546357810628,0.166994209782124,
2.1665910294827));
#11018=CARTESIAN_POINT('Ctrl Pts',(-0.0537908007947409,0.224607784190559,
2.17770574236448));
#11019=CARTESIAN_POINT('Ctrl Pts',(-0.21788513873988,0.0766040070256843,
2.18882045524625));
#11020=CARTESIAN_POINT('Ctrl Pts',(-0.182516369710472,-0.141526955103469,
2.19993516812803));
#11021=CARTESIAN_POINT('Ctrl Pts',(0.0199371177794038,-0.230096980137356,
2.2110498810098));
#11022=CARTESIAN_POINT('Ctrl Pts',(0.204139188235331,-0.108024548875401,
2.22216459389158));
#11023=CARTESIAN_POINT('Ctrl Pts',(0.201461841058376,0.112938992248027,
2.23327930677336));
#11024=CARTESIAN_POINT('Ctrl Pts',(0.0143562266588113,0.230512526239688,
2.24439401965513));
#11025=CARTESIAN_POINT('Ctrl Pts',(-0.185892018555318,0.137063077970044,
2.25550873253691));
#11026=CARTESIAN_POINT('Ctrl Pts',(-0.215964883113702,-0.0818606044959991,
2.26662344541869));
#11027=CARTESIAN_POINT('Ctrl Pts',(-0.0483333206738901,-0.225845423581302,
2.27773815830046));
#11028=CARTESIAN_POINT('Ctrl Pts',(0.16354648179728,-0.163078977908128,
2.28885287118224));
#11029=CARTESIAN_POINT('Ctrl Pts',(0.225704752281254,0.048976482321738,
2.29996758406402));
#11030=CARTESIAN_POINT('Ctrl Pts',(0.0812467689117343,0.216199711180548,
2.31108229694579));
#11031=CARTESIAN_POINT('Ctrl Pts',(-0.137598735282772,0.185496446675884,
2.32219700982757));
#11032=CARTESIAN_POINT('Ctrl Pts',(-0.230460149011143,-0.0150076418454517,
2.33331172270934));
#11033=CARTESIAN_POINT('Ctrl Pts',(-0.112383257382243,-0.201795849986241,
2.34442643559112));
#11034=CARTESIAN_POINT('Ctrl Pts',(0.108644616799776,-0.203806378129441,
2.3555411484729));
#11035=CARTESIAN_POINT('Ctrl Pts',(0.230080867601931,-0.0193251643494075,
2.36665586135467));
#11036=CARTESIAN_POINT('Ctrl Pts',(0.141144990674285,0.18300622889355,2.37777057423645));
#11037=CARTESIAN_POINT('Ctrl Pts',(-0.0775128162224814,0.217492107202628,
2.38888528711823));
#11038=CARTESIAN_POINT('Ctrl Pts',(-0.175202059751607,0.108202911730689,
2.39629509570607));
#11039=CARTESIAN_POINT('Ctrl Pts',(-0.190155688860645,0.0449663651403318,
2.4));
#11040=CARTESIAN_POINT('Ctrl Pts',(0.105793541951255,-0.148236995244729,
-0.0153382721514711));
#11041=CARTESIAN_POINT('Ctrl Pts',(0.155089966961593,-0.11305520139652,
-0.0116333678575457));
#11042=CARTESIAN_POINT('Ctrl Pts',(0.21497519937743,0.00974117628248662,
-0.0042235592696949));
#11043=CARTESIAN_POINT('Ctrl Pts',(0.108183370830488,0.186264075098343,
0.00689115361208128));
#11044=CARTESIAN_POINT('Ctrl Pts',(-0.0977345970672646,0.191720735194958,
0.0180058664938575));
#11045=CARTESIAN_POINT('Ctrl Pts',(-0.214134249288,0.0219430288774403,0.0291205793756336));
#11046=CARTESIAN_POINT('Ctrl Pts',(-0.134529329353402,-0.168066279567892,
0.0402352922574098));
#11047=CARTESIAN_POINT('Ctrl Pts',(0.0682435794252791,-0.204143760009197,
0.0513500051391861));
#11048=CARTESIAN_POINT('Ctrl Pts',(0.208536011121689,-0.0533773322081568,
0.0624647180209621));
#11049=CARTESIAN_POINT('Ctrl Pts',(0.15792760839081,0.146274243875976,0.0735794309027384));
#11050=CARTESIAN_POINT('Ctrl Pts',(-0.0372576226080993,0.212008012654093,
0.0846941437845145));
#11051=CARTESIAN_POINT('Ctrl Pts',(-0.19833434318746,0.083664658915774,
0.0958088566662907));
#11052=CARTESIAN_POINT('Ctrl Pts',(-0.177846277209918,-0.121272589946413,
0.106923569548067));
#11053=CARTESIAN_POINT('Ctrl Pts',(0.00545155897490425,-0.215189173059631,
0.118038282429843));
#11054=CARTESIAN_POINT('Ctrl Pts',(0.183758617328128,-0.112111517639152,
0.129152995311619));
#11055=CARTESIAN_POINT('Ctrl Pts',(0.193843800442202,0.0935991424382365,
0.140267708193395));
#11056=CARTESIAN_POINT('Ctrl Pts',(0.0264745047177667,0.213624172837712,
0.151382421075172));
#11057=CARTESIAN_POINT('Ctrl Pts',(-0.16513087336672,0.138086930438782,
0.162497133956948));
#11058=CARTESIAN_POINT('Ctrl Pts',(-0.205567092178708,-0.0638621501811345,
0.173611846838724));
#11059=CARTESIAN_POINT('Ctrl Pts',(-0.0578167708818694,-0.207348548425574,
0.1847265597205));
#11060=CARTESIAN_POINT('Ctrl Pts',(0.142861949582761,-0.161017594674284,
0.195841272602276));
#11061=CARTESIAN_POINT('Ctrl Pts',(0.212757602765681,0.0327170348815519,
0.206955985484052));
#11062=CARTESIAN_POINT('Ctrl Pts',(0.0878841629903467,0.196500827732778,
0.218070698365829));
#11063=CARTESIAN_POINT('Ctrl Pts',(-0.117442893108306,0.180397806789189,
0.229185411247605));
#11064=CARTESIAN_POINT('Ctrl Pts',(-0.215256773088726,-0.000850510388162502,
0.240300124129381));
#11065=CARTESIAN_POINT('Ctrl Pts',(-0.11601369365937,-0.181320226543997,
0.251414837011157));
#11066=CARTESIAN_POINT('Ctrl Pts',(0.0894342004493663,-0.195800218394246,
0.262529549892933));
#11067=CARTESIAN_POINT('Ctrl Pts',(0.213009494979972,-0.0310347669858385,
0.27364426277471));
#11068=CARTESIAN_POINT('Ctrl Pts',(0.141585102478085,0.16214148285887,0.284758975656486));
#11069=CARTESIAN_POINT('Ctrl Pts',(-0.0594534683484756,0.206885202026802,
0.295873688538262));
#11070=CARTESIAN_POINT('Ctrl Pts',(-0.206065321155091,0.0622357222997597,
0.306988401420038));
#11071=CARTESIAN_POINT('Ctrl Pts',(-0.16403453559407,-0.139387491708681,
0.318103114301814));
#11072=CARTESIAN_POINT('Ctrl Pts',(0.0281617771100779,-0.213408331664074,
0.329217827183591));
#11073=CARTESIAN_POINT('Ctrl Pts',(0.194577371810986,-0.0920643692869703,
0.340332540065367));
#11074=CARTESIAN_POINT('Ctrl Pts',(0.182866979184729,0.113559982550668,
0.351447252947143));
#11075=CARTESIAN_POINT('Ctrl Pts',(0.00375088612404077,0.215225771148598,
0.362561965828919));
#11076=CARTESIAN_POINT('Ctrl Pts',(-0.17879895818941,0.119862981205691,
0.373676678710695));
#11077=CARTESIAN_POINT('Ctrl Pts',(-0.197667174654384,-0.0852284563822003,
0.384791391592471));
#11078=CARTESIAN_POINT('Ctrl Pts',(-0.0355808416787025,-0.212297445624285,
0.395906104474247));
#11079=CARTESIAN_POINT('Ctrl Pts',(0.159077997004871,-0.145018593918386,
0.407020817356024));
#11080=CARTESIAN_POINT('Ctrl Pts',(0.20810877516562,0.0550176281951035,
0.4181355302378));
#11081=CARTESIAN_POINT('Ctrl Pts',(0.0666262335979379,0.204687925168304,
0.429250243119576));
#11082=CARTESIAN_POINT('Ctrl Pts',(-0.135849338819328,0.166976521869098,
0.440364956001352));
#11083=CARTESIAN_POINT('Ctrl Pts',(-0.213961541644003,-0.0235936519104577,
0.451479668883129));
#11084=CARTESIAN_POINT('Ctrl Pts',(-0.0962025056880325,-0.19256500100614,
0.462594381764904));
#11085=CARTESIAN_POINT('Ctrl Pts',(0.109625179512714,-0.185252588996634,
0.473709094646681));
#11086=CARTESIAN_POINT('Ctrl Pts',(0.215096419589165,-0.00835056842810073,
0.484823807528457));
#11087=CARTESIAN_POINT('Ctrl Pts',(0.123657496098414,0.176195985685887,
0.495938520410233));
#11088=CARTESIAN_POINT('Ctrl Pts',(-0.0809837662762514,0.199443804899686,
0.507053233292009));
#11089=CARTESIAN_POINT('Ctrl Pts',(-0.211488384748603,0.0401106573067252,
0.518167946173785));
#11090=CARTESIAN_POINT('Ctrl Pts',(-0.148385817601819,-0.155941818790824,
0.529282659055562));
#11091=CARTESIAN_POINT('Ctrl Pts',(0.0505566471631337,-0.209237250844042,
0.540397371937337));
#11092=CARTESIAN_POINT('Ctrl Pts',(0.203216994906723,-0.0709862993417115,
0.551512084819114));
#11093=CARTESIAN_POINT('Ctrl Pts',(0.169842206486041,0.132249108159955,
0.56262679770089));
#11094=CARTESIAN_POINT('Ctrl Pts',(-0.0190147453460938,0.214416979674124,
0.573741510582666));
#11095=CARTESIAN_POINT('Ctrl Pts',(-0.190464635622116,0.100296681353299,
0.584856223464443));
#11096=CARTESIAN_POINT('Ctrl Pts',(-0.187553545711894,-0.105640282108895,
0.595970936346219));
#11097=CARTESIAN_POINT('Ctrl Pts',(-0.0129464348531298,-0.214868777484641,
0.607085649227995));
#11098=CARTESIAN_POINT('Ctrl Pts',(0.17351249859483,-0.127395504412556,
0.618200362109772));
#11099=CARTESIAN_POINT('Ctrl Pts',(0.20112929722474,0.0767020697962746,
0.629315074991546));
#11100=CARTESIAN_POINT('Ctrl Pts',(0.044622143952873,0.210582682056715,
0.640429787873325));
#11101=CARTESIAN_POINT('Ctrl Pts',(-0.152734381341373,0.15168523484314,
0.651544500755098));
#11102=CARTESIAN_POINT('Ctrl Pts',(-0.210270113385278,-0.0460725637456039,
0.662659213636877));
#11103=CARTESIAN_POINT('Ctrl Pts',(-0.0753139271579653,-0.201653202526504,
0.673773926518651));
#11104=CARTESIAN_POINT('Ctrl Pts',(0.128588444895634,-0.172630279940899,
0.684888639400429));
#11105=CARTESIAN_POINT('Ctrl Pts',(0.214774437636115,0.0144271497961512,
0.696003352282204));
#11106=CARTESIAN_POINT('Ctrl Pts',(0.104345025407248,0.188277235442608,
0.70711806516398));
#11107=CARTESIAN_POINT('Ctrl Pts',(-0.101607111279838,0.189768797884471,
0.718232778045757));
#11108=CARTESIAN_POINT('Ctrl Pts',(-0.214542948858282,0.0175363852701505,
0.729347490927533));
#11109=CARTESIAN_POINT('Ctrl Pts',(-0.131075298026442,-0.170749723163553,
0.740462203809309));
#11110=CARTESIAN_POINT('Ctrl Pts',(0.0723853235080425,-0.202722881426312,
0.751576916691085));
#11111=CARTESIAN_POINT('Ctrl Pts',(0.20958075141886,-0.0491132400464108,
0.762691629572862));
#11112=CARTESIAN_POINT('Ctrl Pts',(0.154915337939347,0.149457150328408,
0.773806342454638));
#11113=CARTESIAN_POINT('Ctrl Pts',(-0.0415674269910586,0.211206890812051,
0.784921055336414));
#11114=CARTESIAN_POINT('Ctrl Pts',(-0.199997262618826,0.0796071394921763,
0.79603576821819));
#11115=CARTESIAN_POINT('Ctrl Pts',(-0.175339468194524,-0.124869021804497,
0.807150481099967));
#11116=CARTESIAN_POINT('Ctrl Pts',(0.00983296161011095,-0.215033752185848,
0.818265193981742));
#11117=CARTESIAN_POINT('Ctrl Pts',(0.186003800022871,-0.108345687916974,
0.829379906863519));
#11118=CARTESIAN_POINT('Ctrl Pts',(0.191897333231851,0.0975275100248876,
0.840494619745294));
#11119=CARTESIAN_POINT('Ctrl Pts',(0.0221183222535954,0.214119082600866,
0.851609332627072));
#11120=CARTESIAN_POINT('Ctrl Pts',(-0.167908921871014,0.134695195420119,
0.862724045508846));
#11121=CARTESIAN_POINT('Ctrl Pts',(-0.204223829299531,-0.0680354999936554,
0.873838758390623));
#11122=CARTESIAN_POINT('Ctrl Pts',(-0.0535818933342823,-0.208483050677661,
0.884953471272399));
#11123=CARTESIAN_POINT('Ctrl Pts',(0.146111623316715,-0.158074650861245,
0.896068184154176));
#11124=CARTESIAN_POINT('Ctrl Pts',(0.212047155054175,0.0370432955685794,
0.907182897035951));
#11125=CARTESIAN_POINT('Ctrl Pts',(0.083863974516331,0.198249931882648,
0.918297609917728));
#11126=CARTESIAN_POINT('Ctrl Pts',(-0.121092538515599,0.177968533255176,
0.929412322799505));
#11127=CARTESIAN_POINT('Ctrl Pts',(-0.21519480482684,-0.00523428015002993,
0.940527035681279));
#11128=CARTESIAN_POINT('Ctrl Pts',(-0.112296840738152,-0.183645368232854,
0.951641748563058));
#11129=CARTESIAN_POINT('Ctrl Pts',(0.0934033425602478,-0.193938179097679,
0.962756461444831));
#11130=CARTESIAN_POINT('Ctrl Pts',(0.213597372402487,-0.0266901520397281,
0.97387117432661));
#11131=CARTESIAN_POINT('Ctrl Pts',(0.138253542443842,0.164991392850898,
0.984985887208384));
#11132=CARTESIAN_POINT('Ctrl Pts',(-0.0636545869501867,0.205631454970663,
0.996100600090161));
#11133=CARTESIAN_POINT('Ctrl Pts',(-0.207290081438881,0.0580260618189137,
1.00721531297194));
#11134=CARTESIAN_POINT('Ctrl Pts',(-0.161161729927952,-0.142699329079643,
1.01833002585371));
#11135=CARTESIAN_POINT('Ctrl Pts',(0.0325022368270573,-0.21279052214417,
1.02944473873549));
#11136=CARTESIAN_POINT('Ctrl Pts',(0.196412008778918,-0.0880824870254049,
1.04055945161727));
#11137=CARTESIAN_POINT('Ctrl Pts',(0.180516273744238,0.117260720732245,
1.05167416449904));
#11138=CARTESIAN_POINT('Ctrl Pts',(-0.000633206831217092,0.215257521964412,
1.06278887738082));
#11139=CARTESIAN_POINT('Ctrl Pts',(-0.181203017782488,0.116196678350416,
1.0739035902626));
#11140=CARTESIAN_POINT('Ctrl Pts',(-0.195890402896217,-0.089236493467125,
1.08501830314437));
#11141=CARTESIAN_POINT('Ctrl Pts',(-0.03124978548339,-0.212978056664043,
1.09613301602615));
#11142=CARTESIAN_POINT('Ctrl Pts',(0.161998469298423,-0.14174871307394,
1.10724772890792));
#11143=CARTESIAN_POINT('Ctrl Pts',(0.206945115210521,0.0592445862814022,
1.1183624417897));
#11144=CARTESIAN_POINT('Ctrl Pts',(0.0624437146913072,0.20600238884222,
1.12947715467148));
#11145=CARTESIAN_POINT('Ctrl Pts',(-0.13922182690052,0.164175164466591,
1.14059186755325));
#11146=CARTESIAN_POINT('Ctrl Pts',(-0.213436652392715,-0.0279463258504929,
1.15170658043503));
#11147=CARTESIAN_POINT('Ctrl Pts',(-0.0922607493262528,-0.194484333165705,
1.1628212933168));
#11148=CARTESIAN_POINT('Ctrl Pts',(0.113375319443406,-0.182981525445211,
1.17393600619858));
#11149=CARTESIAN_POINT('Ctrl Pts',(0.215221874939318,-0.00396815583804349,
1.18505071908036));
#11150=CARTESIAN_POINT('Ctrl Pts',(0.120043418682428,0.178677864729199,
1.19616543196213));
#11151=CARTESIAN_POINT('Ctrl Pts',(-0.0850288668305293,0.197753112538505,
1.20728014484391));
#11152=CARTESIAN_POINT('Ctrl Pts',(-0.212261418388302,0.0357951390126765,
1.21839485772569));
#11153=CARTESIAN_POINT('Ctrl Pts',(-0.145179110155855,-0.158931518861127,
1.22950957060746));
#11154=CARTESIAN_POINT('Ctrl Pts',(0.0548075131829614,-0.208164209728402,
1.24062428348924));
#11155=CARTESIAN_POINT('Ctrl Pts',(0.204620561312197,-0.0668328332590501,
1.25173899637101));
#11156=CARTESIAN_POINT('Ctrl Pts',(0.167113577456916,0.135680705860126,
1.26285370925279));
#11157=CARTESIAN_POINT('Ctrl Pts',(-0.0233776445097808,0.213985250543875,
1.27396842213457));
#11158=CARTESIAN_POINT('Ctrl Pts',(-0.192467785914425,0.0963968521184676,
1.28508313501634));
#11159=CARTESIAN_POINT('Ctrl Pts',(-0.185363161835691,-0.1094381101236,
1.29619784789812));
#11160=CARTESIAN_POINT('Ctrl Pts',(-0.00856770521723566,-0.215087880040835,
1.30731256077989));
#11161=CARTESIAN_POINT('Ctrl Pts',(0.17607106296793,-0.123835303926197,
1.31842727366167));
#11162=CARTESIAN_POINT('Ctrl Pts',(0.199525456840005,0.0807823853692007,
1.32954198654345));
#11163=CARTESIAN_POINT('Ctrl Pts',(0.0403241355810343,0.211447785050572,
1.34065669942522));
#11164=CARTESIAN_POINT('Ctrl Pts',(-0.155791943013894,0.148543166133976,
1.351771412307));
#11165=CARTESIAN_POINT('Ctrl Pts',(-0.209288181446391,-0.0503453952215415,
1.36288612518877));
#11166=CARTESIAN_POINT('Ctrl Pts',(-0.0711914118687858,-0.203145230289267,
1.37400083807055));
#11167=CARTESIAN_POINT('Ctrl Pts',(0.132077584110531,-0.169975626160565,
1.38511555095233));
#11168=CARTESIAN_POINT('Ctrl Pts',(0.214436065910022,0.0187982805113507,
1.39623026383411));
#11169=CARTESIAN_POINT('Ctrl Pts',(0.100488905366888,0.190363288507304,
1.40734497671588));
#11170=CARTESIAN_POINT('Ctrl Pts',(-0.105450891921556,0.187660094602179,
1.41845968959766));
#11171=CARTESIAN_POINT('Ctrl Pts',(-0.214855598499328,0.0131633394944521,
1.42957440247943));
#11172=CARTESIAN_POINT('Ctrl Pts',(-0.127570601340334,-0.173383803703852,
1.44068911536121));
#11173=CARTESIAN_POINT('Ctrl Pts',(0.0764989895569963,-0.201206625909559,
1.45180382824298));
#11174=CARTESIAN_POINT('Ctrl Pts',(0.210537528449068,-0.0448347056163908,
1.46291854112476));
#11175=CARTESIAN_POINT('Ctrl Pts',(0.151839343767946,0.152581176418554,
1.47403325400654));
#11176=CARTESIAN_POINT('Ctrl Pts',(-0.0458602714083437,0.210316516753924,
1.48514796688831));
#11177=CARTESIAN_POINT('Ctrl Pts',(-0.201577069941283,0.0755174588226969,
1.49626267977009));
#11178=CARTESIAN_POINT('Ctrl Pts',(-0.172760002734623,-0.128414108135685,
1.50737739265187));
#11179=CARTESIAN_POINT('Ctrl Pts',(0.0142103264432017,-0.214788892486386,
1.51849210553364));
#11180=CARTESIAN_POINT('Ctrl Pts',(0.18817180261632,-0.104535039165226,
1.52960681841542));
#11181=CARTESIAN_POINT('Ctrl Pts',(0.189871274137357,0.101415486838092,
1.54072153129719));
#11182=CARTESIAN_POINT('Ctrl Pts',(0.0177529586468273,0.214525136458259,
1.55183624417897));
#11183=CARTESIAN_POINT('Ctrl Pts',(-0.170617314908023,0.131247604041854,
1.56295095706075));
#11184=CARTESIAN_POINT('Ctrl Pts',(-0.202795851519484,-0.0721806367361637,
1.57406566994252));
#11185=CARTESIAN_POINT('Ctrl Pts',(-0.049324787966875,-0.209531064535007,
1.5851803828243));
#11186=CARTESIAN_POINT('Ctrl Pts',(0.149300686268282,-0.155066136835127,
1.59629509570608));
#11187=CARTESIAN_POINT('Ctrl Pts',(0.211248745742492,0.0413541912673223,
1.60740980858785));
#11188=CARTESIAN_POINT('Ctrl Pts',(0.0798089972886537,0.199916796855417,
1.61852452146963));
#11189=CARTESIAN_POINT('Ctrl Pts',(-0.124691951999022,0.175465434829268,
1.6296392343514));
#11190=CARTESIAN_POINT('Ctrl Pts',(-0.215043569045195,-0.00961587881864149,
1.64075394723318));
#11191=CARTESIAN_POINT('Ctrl Pts',(-0.108533404590579,-0.185894329663731,
1.65186866011496));
#11192=CARTESIAN_POINT('Ctrl Pts',(0.0973337388935138,-0.19199569001975,
1.66298337299673));
#11193=CARTESIAN_POINT('Ctrl Pts',(0.214096644925695,-0.0223344654001731,
1.67409808587851));
#11194=CARTESIAN_POINT('Ctrl Pts',(0.134864631786142,0.167772860756258,
1.68521279876028));
#11195=CARTESIAN_POINT('Ctrl Pts',(-0.0678293002229216,0.204292407456614,
1.69632751164206));
#11196=CARTESIAN_POINT('Ctrl Pts',(-0.208428853222539,0.0537923308426739,
1.70744222452384));
#11197=CARTESIAN_POINT('Ctrl Pts',(-0.158222070818878,-0.14595197161716,
1.71855693740561));
#11198=CARTESIAN_POINT('Ctrl Pts',(0.0368292138986469,-0.212084442420368,
1.72967165028739));
#11199=CARTESIAN_POINT('Ctrl Pts',(0.198165169710719,-0.0840640662035352,
1.74078636316916));
#11200=CARTESIAN_POINT('Ctrl Pts',(0.178090686169176,0.120912816578486,
1.75190107605094));
#11201=CARTESIAN_POINT('Ctrl Pts',(-0.00501703711827952,0.215199979209349,
1.76301578893272));
#11202=CARTESIAN_POINT('Ctrl Pts',(-0.183531910364484,0.112482174548297,
1.77413050181449));
#11203=CARTESIAN_POINT('Ctrl Pts',(-0.194032371475433,-0.0932075132849812,
1.78524521469627));
#11204=CARTESIAN_POINT('Ctrl Pts',(-0.0269057661873462,-0.213570319705296,
1.79635992757805));
#11205=CARTESIAN_POINT('Ctrl Pts',(0.164851741051457,-0.138420031734765,
1.80747464045982));
#11206=CARTESIAN_POINT('Ctrl Pts',(0.205695609854155,0.0634469684057254,
1.8185893533416));
#11207=CARTESIAN_POINT('Ctrl Pts',(0.0582352927536283,0.207231398178581,
1.82970406622338));
#11208=CARTESIAN_POINT('Ctrl Pts',(-0.142536562695159,0.161305703582358,
1.84081877910515));
#11209=CARTESIAN_POINT('Ctrl Pts',(-0.212823224907265,-0.0322874070377658,
1.85193349198693));
#11210=CARTESIAN_POINT('Ctrl Pts',(-0.0882807211693674,-0.196322988931421,
1.8630482048687));
#11211=CARTESIAN_POINT('Ctrl Pts',(0.117078428789294,-0.180634557118456,
1.87416291775048));
#11212=CARTESIAN_POINT('Ctrl Pts',(0.215258051505596,0.000415902830639266,
1.88527763063225));
#11213=CARTESIAN_POINT('Ctrl Pts',(0.116379544606898,0.181085624250633,
1.89639234351403));
#11214=CARTESIAN_POINT('Ctrl Pts',(-0.0890386955341811,0.195980387821644,
1.90750705639581));
#11215=CARTESIAN_POINT('Ctrl Pts',(-0.212946401306843,0.0314647721049302,
1.91862176927758));
#11216=CARTESIAN_POINT('Ctrl Pts',(-0.141912179210756,-0.16185529062964,
1.92973648215936));
#11217=CARTESIAN_POINT('Ctrl Pts',(0.0590356438366701,-0.207004817504183,
1.94085119504114));
#11218=CARTESIAN_POINT('Ctrl Pts',(0.205939246592667,-0.062651643442089,
1.95196590792291));
#11219=CARTESIAN_POINT('Ctrl Pts',(0.16431562602751,0.139056020208906,1.96308062080469));
#11220=CARTESIAN_POINT('Ctrl Pts',(-0.0277308461105627,0.213464755608839,
1.97419533368647));
#11221=CARTESIAN_POINT('Ctrl Pts',(-0.194391096321177,0.092457035341819,
1.98531004656824));
#11222=CARTESIAN_POINT('Ctrl Pts',(-0.183095885228843,-0.113190540794836,
1.99642475945002));
#11223=CARTESIAN_POINT('Ctrl Pts',(-0.00418542150807707,-0.215217759397172,
2.00753947233179));
#11224=CARTESIAN_POINT('Ctrl Pts',(0.178556589177984,-0.12022373382265,
2.01865418521357));
#11225=CARTESIAN_POINT('Ctrl Pts',(0.1978388488922,0.0848291906258296,2.02976889809535));
#11226=CARTESIAN_POINT('Ctrl Pts',(0.0360093998674796,0.212225174836164,
2.04088361097712));
#11227=CARTESIAN_POINT('Ctrl Pts',(-0.158784878749449,0.145339478441341,
2.0519983238589));
#11228=CARTESIAN_POINT('Ctrl Pts',(-0.208219432151661,-0.0545973423170097,
2.06311303674067));
#11229=CARTESIAN_POINT('Ctrl Pts',(-0.0670393648087706,-0.204552988925698,
2.07422774962245));
#11230=CARTESIAN_POINT('Ctrl Pts',(0.135511934624805,-0.167250462741263,
2.08534246250422));
#11231=CARTESIAN_POINT('Ctrl Pts',(0.214008741377946,0.0231616132892584,
2.09645717538601));
#11232=CARTESIAN_POINT('Ctrl Pts',(0.0965911002974415,0.192370374670147,
2.10757188826778));
#11233=CARTESIAN_POINT('Ctrl Pts',(-0.109250929180699,0.185473545786568,
2.11868660114956));
#11234=CARTESIAN_POINT('Ctrl Pts',(-0.215079121344005,0.00878483324502261,
2.12980131403133));
#11235=CARTESIAN_POINT('Ctrl Pts',(-0.124012985461959,-0.175945960758605,
2.14091602691311));
#11236=CARTESIAN_POINT('Ctrl Pts',(0.0805809219631423,-0.199606905552042,
2.15203073979489));
#11237=CARTESIAN_POINT('Ctrl Pts',(0.211406970195834,-0.0405375725545616,
2.16314545267666));
#11238=CARTESIAN_POINT('Ctrl Pts',(0.14870036265752,0.15564190807653,2.17426016555844));
#11239=CARTESIAN_POINT('Ctrl Pts',(-0.0501340907782409,0.209338899509574,
2.18537487844021));
#11240=CARTESIAN_POINT('Ctrl Pts',(-0.203073260918684,0.0713964504238905,
2.19648959132199));
#11241=CARTESIAN_POINT('Ctrl Pts',(-0.170108868289522,-0.131905922758067,
2.20760430420376));
#11242=CARTESIAN_POINT('Ctrl Pts',(0.0185817882954204,-0.214454938754768,
2.21871901708554));
#11243=CARTESIAN_POINT('Ctrl Pts',(0.190261763037141,-0.100681017192216,
2.22983372996732));
#11244=CARTESIAN_POINT('Ctrl Pts',(0.187766422487623,0.105261375664803,
2.24094844284909));
#11245=CARTESIAN_POINT('Ctrl Pts',(0.0133802873337488,0.214842235945161,
2.25206315573087));
#11246=CARTESIAN_POINT('Ctrl Pts',(-0.173255039811833,0.12774550093643,
2.26317786861264));
#11247=CARTESIAN_POINT('Ctrl Pts',(-0.201283544676172,-0.0762957032862286,
2.27429258149442));
#11248=CARTESIAN_POINT('Ctrl Pts',(-0.0450476113104433,-0.210492403912733,
2.2854072943762));
#11249=CARTESIAN_POINT('Ctrl Pts',(0.152428557369401,-0.15199283449353,
2.29652200725797));
#11250=CARTESIAN_POINT('Ctrl Pts',(0.21036129547742,0.0456470506934145,
2.30763672013975));
#11251=CARTESIAN_POINT('Ctrl Pts',(0.0757235963748345,0.201502409081358,
2.31875143302153));
#11252=CARTESIAN_POINT('Ctrl Pts',(-0.128244744151725,0.172886358992444,
2.3298661459033));
#11253=CARTESIAN_POINT('Ctrl Pts',(-0.214793419331693,-0.0139874191781991,
2.34098085878508));
#11254=CARTESIAN_POINT('Ctrl Pts',(-0.104743419772758,-0.188077725417916,
2.35209557166686));
#11255=CARTESIAN_POINT('Ctrl Pts',(0.101258932767922,-0.189951577432652,
2.36321028454863));
#11256=CARTESIAN_POINT('Ctrl Pts',(0.214439921552908,-0.0180114355890496,
2.37432499743041));
#11257=CARTESIAN_POINT('Ctrl Pts',(0.131549924351581,0.170565426741709,
2.38543971031219));
#11258=CARTESIAN_POINT('Ctrl Pts',(-0.0722434785792406,0.202706947748475,
2.39655442319396));
#11259=CARTESIAN_POINT('Ctrl Pts',(-0.163291786668867,0.100847254902872,
2.40396423178181));
#11260=CARTESIAN_POINT('Ctrl Pts',(-0.177228864907903,0.0419095421262742,
2.40766913607574));
#11261=CARTESIAN_POINT('Ctrl Pts',(0.0980771099081341,-0.137424797458509,
-0.00766913607573553));
#11262=CARTESIAN_POINT('Ctrl Pts',(0.143777923064053,-0.104809114134417,
-0.00396423178181014));
#11263=CARTESIAN_POINT('Ctrl Pts',(0.199295210917303,0.00903066859536452,
0.00344557680604064));
#11264=CARTESIAN_POINT('Ctrl Pts',(0.10029262803266,0.172678235631573,0.0145602896878168));
#11265=CARTESIAN_POINT('Ctrl Pts',(-0.090605973120834,0.177736894621117,
0.025675002569593));
#11266=CARTESIAN_POINT('Ctrl Pts',(-0.198515598543739,0.0203425352364337,
0.0367897154513692));
#11267=CARTESIAN_POINT('Ctrl Pts',(-0.124716949423446,-0.155807761693303,
0.0479044283331453));
#11268=CARTESIAN_POINT('Ctrl Pts',(0.0632659887963794,-0.189253801491094,
0.0590191412149216));
#11269=CARTESIAN_POINT('Ctrl Pts',(0.193325687989632,-0.0494840647267017,
0.0701338540966976));
#11270=CARTESIAN_POINT('Ctrl Pts',(0.146408590921473,0.135605206411971,
0.081248566978474));
#11271=CARTESIAN_POINT('Ctrl Pts',(-0.0345401040560084,0.196544446617184,
0.0923632798602499));
#11272=CARTESIAN_POINT('Ctrl Pts',(-0.183868115355446,0.0775622764543633,
0.103477992742026));
#11273=CARTESIAN_POINT('Ctrl Pts',(-0.164874420072892,-0.112427137929636,
0.114592705623802));
#11274=CARTESIAN_POINT('Ctrl Pts',(0.00505392993646349,-0.199493577660297,
0.125707418505579));
#11275=CARTESIAN_POINT('Ctrl Pts',(0.170355522424629,-0.103934261342056,
0.136822131387355));
#11276=CARTESIAN_POINT('Ctrl Pts',(0.179705106477489,0.0867721527317011,
0.147936844269131));
#11277=CARTESIAN_POINT('Ctrl Pts',(0.0245434916071218,0.19804272635179,
0.159051557150907));
#11278=CARTESIAN_POINT('Ctrl Pts',(-0.153086459888794,0.128015064093063,
0.170166270032684));
#11279=CARTESIAN_POINT('Ctrl Pts',(-0.190573317815533,-0.0592041348343418,
0.181280982914459));
#11280=CARTESIAN_POINT('Ctrl Pts',(-0.0535996969921641,-0.19222483715119,
0.192395695796236));
#11281=CARTESIAN_POINT('Ctrl Pts',(0.132441800061622,-0.149273197954655,
0.203510408678012));
#11282=CARTESIAN_POINT('Ctrl Pts',(0.197239362681098,0.0303307004072554,
0.214625121559788));
#11283=CARTESIAN_POINT('Ctrl Pts',(0.0814740158407841,0.182168333937314,
0.225739834441564));
#11284=CARTESIAN_POINT('Ctrl Pts',(-0.108876773788515,0.167239844675987,
0.23685454732334));
#11285=CARTESIAN_POINT('Ctrl Pts',(-0.199556247038418,-0.000788475357558915,
0.247969260205116));
#11286=CARTESIAN_POINT('Ctrl Pts',(-0.10755181813576,-0.168094984432202,
0.259083973086893));
#11287=CARTESIAN_POINT('Ctrl Pts',(0.0829109957492487,-0.181518826057814,
0.270198685968668));
#11288=CARTESIAN_POINT('Ctrl Pts',(0.197472882231822,-0.0287711347640326,
0.281313398850446));
#11289=CARTESIAN_POINT('Ctrl Pts',(0.131258084387575,0.150315111316951,
0.292428111732221));
#11290=CARTESIAN_POINT('Ctrl Pts',(-0.0551170160492373,0.191795286586576,
0.303542824613998));
#11291=CARTESIAN_POINT('Ctrl Pts',(-0.191035206671645,0.0576963363134077,
0.314657537495773));
#11292=CARTESIAN_POINT('Ctrl Pts',(-0.152070087450166,-0.129220764254499,
0.32577225037755));
#11293=CARTESIAN_POINT('Ctrl Pts',(0.0261076967260043,-0.197842628329557,
0.336886963259326));
#11294=CARTESIAN_POINT('Ctrl Pts',(0.180385172183149,-0.0853493237738671,
0.348001676141102));
#11295=CARTESIAN_POINT('Ctrl Pts',(0.169528919112412,0.105277077261666,
0.359116389022878));
#11296=CARTESIAN_POINT('Ctrl Pts',(0.00347730176961437,0.199527506336167,
0.370231101904654));
#11297=CARTESIAN_POINT('Ctrl Pts',(-0.165757613842657,0.111120344066412,
0.381345814786431));
#11298=CARTESIAN_POINT('Ctrl Pts',(-0.18324960915612,-0.079012012734662,
0.392460527668206));
#11299=CARTESIAN_POINT('Ctrl Pts',(-0.0329856251675023,-0.196812768753913,
0.403575240549983));
#11300=CARTESIAN_POINT('Ctrl Pts',(0.147475071809217,-0.134441141794937,
0.414689953431759));
#11301=CARTESIAN_POINT('Ctrl Pts',(0.192929614022855,0.0510047198331068,
0.425804666313535));
#11302=CARTESIAN_POINT('Ctrl Pts',(0.0617666098972408,0.189758276009417,
0.436919379195312));
#11303=CARTESIAN_POINT('Ctrl Pts',(-0.125940679256865,0.154797489387205,
0.448034092077088));
#11304=CARTESIAN_POINT('Ctrl Pts',(-0.198355487952206,-0.0218727641487044,
0.459148804958864));
#11305=CARTESIAN_POINT('Ctrl Pts',(-0.0891856303303566,-0.178519580872352,
0.47026351784064));
#11306=CARTESIAN_POINT('Ctrl Pts',(0.101629273218976,-0.171740525902436,
0.481378230722416));
#11307=CARTESIAN_POINT('Ctrl Pts',(0.199407589497414,-0.00774148972057319,
0.492492943604193));
#11308=CARTESIAN_POINT('Ctrl Pts',(0.114638092383726,0.163344498489797,
0.503607656485968));
#11309=CARTESIAN_POINT('Ctrl Pts',(-0.0750769243505434,0.184896654491977,
0.514722369367745));
#11310=CARTESIAN_POINT('Ctrl Pts',(-0.196062719639731,0.037185042419435,
0.525837082249521));
#11311=CARTESIAN_POINT('Ctrl Pts',(-0.137562764922345,-0.144567642019861,
0.536951795131298));
#11312=CARTESIAN_POINT('Ctrl Pts',(0.046869116478677,-0.193975780273649,
0.548066508013073));
#11313=CARTESIAN_POINT('Ctrl Pts',(0.188394633330749,-0.0658086585825549,
0.559181220894849));
#11314=CARTESIAN_POINT('Ctrl Pts',(0.157454155001704,0.12260304435438,0.570295933776627));
#11315=CARTESIAN_POINT('Ctrl Pts',(-0.0176278365842307,0.198777706973449,
0.581410646658401));
#11316=CARTESIAN_POINT('Ctrl Pts',(-0.176572413183126,0.0929811825852432,
0.592525359540179));
#11317=CARTESIAN_POINT('Ctrl Pts',(-0.173873654073534,-0.0979350286229587,
0.603640072421953));
#11318=CARTESIAN_POINT('Ctrl Pts',(-0.0120021401173466,-0.199196551287582,
0.614754785303731));
#11319=CARTESIAN_POINT('Ctrl Pts',(0.160856741170093,-0.118103455632765,
0.625869498185506));
#11320=CARTESIAN_POINT('Ctrl Pts',(0.186459209379211,0.0711075287852313,
0.636984211067283));
#11321=CARTESIAN_POINT('Ctrl Pts',(0.0413674675796324,0.195223077627392,
0.648098923949059));
#11322=CARTESIAN_POINT('Ctrl Pts',(-0.141594150543432,0.140621527314088,
0.659213636830835));
#11323=CARTESIAN_POINT('Ctrl Pts',(-0.194933307274904,-0.0427120957941727,
0.670328349712612));
#11324=CARTESIAN_POINT('Ctrl Pts',(-0.0698206353171251,-0.18694490176567,
0.681443062594386));
#11325=CARTESIAN_POINT('Ctrl Pts',(0.119209384716092,-0.160038870303041,
0.692557775476165));
#11326=CARTESIAN_POINT('Ctrl Pts',(0.199109092454823,0.0133748537965563,
0.703672488357939));
#11327=CARTESIAN_POINT('Ctrl Pts',(0.0967342461220328,0.174544558893895,
0.714787201239717));
#11328=CARTESIAN_POINT('Ctrl Pts',(-0.0941960315973934,0.175927328870661,
0.725901914121491));
#11329=CARTESIAN_POINT('Ctrl Pts',(-0.198894488142619,0.016257306011409,
0.73701662700327));
#11330=CARTESIAN_POINT('Ctrl Pts',(-0.121514850279847,-0.158295478690104,
0.748131339885044));
#11331=CARTESIAN_POINT('Ctrl Pts',(0.0671056398953447,-0.187936559792125,
0.759246052766821));
#11332=CARTESIAN_POINT('Ctrl Pts',(0.194294226400023,-0.0455309894454271,
0.770360765648596));
#11333=CARTESIAN_POINT('Ctrl Pts',(0.143616031236901,0.138555956147776,
0.781475478530374));
#11334=CARTESIAN_POINT('Ctrl Pts',(-0.0385355573734222,0.195801757474703,
0.792590191412148));
#11335=CARTESIAN_POINT('Ctrl Pts',(-0.185409743784085,0.0738007067864724,
0.803704904293926));
#11336=CARTESIAN_POINT('Ctrl Pts',(-0.162550454178691,-0.11576125111005,
0.814819617175701));
#11337=CARTESIAN_POINT('Ctrl Pts',(0.00911575923038187,-0.199349492966289,
0.825934330057478));
#11338=CARTESIAN_POINT('Ctrl Pts',(0.172436944653762,-0.100443105939323,
0.837049042939254));
#11339=CARTESIAN_POINT('Ctrl Pts',(0.177900611845764,0.0904139907158485,
0.84816375582103));
#11340=CARTESIAN_POINT('Ctrl Pts',(0.0205050429604615,0.198501538093417,
0.859278468702807));
#11341=CARTESIAN_POINT('Ctrl Pts',(-0.155661881445351,0.124870717452717,
0.870393181584582));
#11342=CARTESIAN_POINT('Ctrl Pts',(-0.18932803064009,-0.063073086385622,
0.881507894466359));
#11343=CARTESIAN_POINT('Ctrl Pts',(-0.0496737054522119,-0.193276590405847,
0.892622607348134));
#11344=CARTESIAN_POINT('Ctrl Pts',(0.13545444716741,-0.14654490832108,0.903737320229911));
#11345=CARTESIAN_POINT('Ctrl Pts',(0.196580734025697,0.0343414097290811,
0.914852033111688));
#11346=CARTESIAN_POINT('Ctrl Pts',(0.0777470542555572,0.183789860892396,
0.925966745993463));
#11347=CARTESIAN_POINT('Ctrl Pts',(-0.112260219196759,0.164987758934287,
0.93708145887524));
#11348=CARTESIAN_POINT('Ctrl Pts',(-0.199498798654332,-0.00485249912325078,
0.948196171757015));
#11349=CARTESIAN_POINT('Ctrl Pts',(-0.104106067235061,-0.170250533558963,
0.959310884638792));
#11350=CARTESIAN_POINT('Ctrl Pts',(0.0865906342212202,-0.179792601286676,
0.970425597520567));
#11351=CARTESIAN_POINT('Ctrl Pts',(0.198017880702589,-0.0247434099169477,
0.981540310402345));
#11352=CARTESIAN_POINT('Ctrl Pts',(0.128169523652984,0.152957152885473,
0.992655023284119));
#11353=CARTESIAN_POINT('Ctrl Pts',(-0.0590117109733095,0.190632986076034,
1.0037697361659));
#11354=CARTESIAN_POINT('Ctrl Pts',(-0.192170634664213,0.0537937225428421,
1.01488444904767));
#11355=CARTESIAN_POINT('Ctrl Pts',(-0.149406820185795,-0.132291040869109,
1.02599916192945));
#11356=CARTESIAN_POINT('Ctrl Pts',(0.0301315694205225,-0.197269880966454,
1.03711387481122));
#11357=CARTESIAN_POINT('Ctrl Pts',(0.182085993312934,-0.0816578743998708,
1.048228587693));
#11358=CARTESIAN_POINT('Ctrl Pts',(0.16734967081808,0.108707888809153,1.05934330057478));
#11359=CARTESIAN_POINT('Ctrl Pts',(-0.000587021616197327,0.199556941292166,
1.07045801345656));
#11360=CARTESIAN_POINT('Ctrl Pts',(-0.167986324712783,0.107721456180996,
1.08157272633833));
#11361=CARTESIAN_POINT('Ctrl Pts',(-0.181602432629148,-0.0827277092360154,
1.09268743922011));
#11362=CARTESIAN_POINT('Ctrl Pts',(-0.0289704701150162,-0.197443736982406,
1.10380215210188));
#11363=CARTESIAN_POINT('Ctrl Pts',(0.150182528964309,-0.131409761456854,
1.11491686498366));
#11364=CARTESIAN_POINT('Ctrl Pts',(0.191850829787004,0.0549233695461304,
1.12603157786543));
#11365=CARTESIAN_POINT('Ctrl Pts',(0.0578891580326697,0.190976864553096,
1.13714629074721));
#11366=CARTESIAN_POINT('Ctrl Pts',(-0.129067182804268,0.152200459050663,
1.14826100362899));
#11367=CARTESIAN_POINT('Ctrl Pts',(-0.197868883384114,-0.025907960178041,
1.15937571651076));
#11368=CARTESIAN_POINT('Ctrl Pts',(-0.0855313801294934,-0.180298919645701,
1.17049042939254));
#11369=CARTESIAN_POINT('Ctrl Pts',(0.10510588322153,-0.169635110529881,
1.18160514227432));
#11370=CARTESIAN_POINT('Ctrl Pts',(0.199523894310908,-0.00367872413648953,
1.19271985515609));
#11371=CARTESIAN_POINT('Ctrl Pts',(0.111287620687565,0.165645352768991,
1.20383456803787));
#11372=CARTESIAN_POINT('Ctrl Pts',(-0.0788269809639628,0.183329278851933,
1.21494928091964));
#11373=CARTESIAN_POINT('Ctrl Pts',(-0.196779369293813,0.0331842919555645,
1.22606399380142));
#11374=CARTESIAN_POINT('Ctrl Pts',(-0.134589950203975,-0.147339277575106,
1.2371787066832));
#11375=CARTESIAN_POINT('Ctrl Pts',(0.0508099303142088,-0.192981005266653,
1.24829341956497));
#11376=CARTESIAN_POINT('Ctrl Pts',(0.189695825578159,-0.0619581404698651,
1.25940813244675));
#11377=CARTESIAN_POINT('Ctrl Pts',(0.154924548333356,0.125784346148352,
1.27052284532852));
#11378=CARTESIAN_POINT('Ctrl Pts',(-0.021672512023798,0.198377467558292,
1.2816375582103));
#11379=CARTESIAN_POINT('Ctrl Pts',(-0.178429456512593,0.089365801405703,
1.29275227109208));
#11380=CARTESIAN_POINT('Ctrl Pts',(-0.171843033714247,-0.101455848407801,
1.30386698397385));
#11381=CARTESIAN_POINT('Ctrl Pts',(-0.00794278885793319,-0.199399672811719,
1.31498169685563));
#11382=CARTESIAN_POINT('Ctrl Pts',(0.163228687459056,-0.114802931158818,
1.32609640973741));
#11383=CARTESIAN_POINT('Ctrl Pts',(0.184972350854696,0.0748902318834049,
1.33721112261918));
#11384=CARTESIAN_POINT('Ctrl Pts',(0.0373829498888915,0.196025081226529,
1.34832583550096));
#11385=CARTESIAN_POINT('Ctrl Pts',(-0.144428697971146,0.137708636674038,
1.35944054838274));
#11386=CARTESIAN_POINT('Ctrl Pts',(-0.194022996069548,-0.0466732729563628,
1.37055526126451));
#11387=CARTESIAN_POINT('Ctrl Pts',(-0.0659988104906048,-0.18832810312348,
1.38166997414629));
#11388=CARTESIAN_POINT('Ctrl Pts',(0.122444031027697,-0.157577843232959,
1.39278468702806));
#11389=CARTESIAN_POINT('Ctrl Pts',(0.198795401086165,0.0174271603898547,
1.40389939990984));
#11390=CARTESIAN_POINT('Ctrl Pts',(0.0931593860498409,0.17647845818422,
1.41501411279162));
#11391=CARTESIAN_POINT('Ctrl Pts',(-0.0977594522893137,0.173972431437732,
1.42612882567339));
#11392=CARTESIAN_POINT('Ctrl Pts',(-0.199184333558908,0.0122032240394291,
1.43724353855517));
#11393=CARTESIAN_POINT('Ctrl Pts',(-0.118265781237084,-0.160737433103322,
1.44835825143694));
#11394=CARTESIAN_POINT('Ctrl Pts',(0.070919260932766,-0.1865308978186,1.45947296431872));
#11395=CARTESIAN_POINT('Ctrl Pts',(0.195181217460332,-0.0415645252945986,
1.47058767720049));
#11396=CARTESIAN_POINT('Ctrl Pts',(0.140764395750831,0.141452120172044,
1.48170239008227));
#11397=CARTESIAN_POINT('Ctrl Pts',(-0.042515287761186,0.194976326047155,
1.49281710296405));
#11398=CARTESIAN_POINT('Ctrl Pts',(-0.186874322184056,0.0700093216687068,
1.50393181584582));
#11399=CARTESIAN_POINT('Ctrl Pts',(-0.160159131298779,-0.119047763834031,
1.5150465287276));
#11400=CARTESIAN_POINT('Ctrl Pts',(0.0131738452337871,-0.19912249298866,
1.52616124160938));
#11401=CARTESIAN_POINT('Ctrl Pts',(0.174446816189558,-0.0969104005439529,
1.53727595449115));
#11402=CARTESIAN_POINT('Ctrl Pts',(0.176022330649899,0.0940183839727135,
1.54839066737293));
#11403=CARTESIAN_POINT('Ctrl Pts',(0.0164580828308227,0.198877974953982,
1.55950538025471));
#11404=CARTESIAN_POINT('Ctrl Pts',(-0.158172728106364,0.121674588537019,
1.57062009313648));
#11405=CARTESIAN_POINT('Ctrl Pts',(-0.188004207549408,-0.0669158826885055,
1.58173480601826));
#11406=CARTESIAN_POINT('Ctrl Pts',(-0.0457271073583309,-0.194248163607542,
1.59284951890003));
#11407=CARTESIAN_POINT('Ctrl Pts',(0.138410904355969,-0.143755831073476,
1.60396423178181));
#11408=CARTESIAN_POINT('Ctrl Pts',(0.19584055956543,0.038337874763241,1.61507894466359));
#11409=CARTESIAN_POINT('Ctrl Pts',(0.0739878413593942,0.185335147080201,
1.62619365754536));
#11410=CARTESIAN_POINT('Ctrl Pts',(-0.115597096526957,0.162667232984398,
1.63730837042714));
#11411=CARTESIAN_POINT('Ctrl Pts',(-0.199358593797733,-0.00891451015217326,
1.64842308330891));
#11412=CARTESIAN_POINT('Ctrl Pts',(-0.100617130822971,-0.172335458908536,
1.65953779619069));
#11413=CARTESIAN_POINT('Ctrl Pts',(0.0902343529780598,-0.177991794627994,
1.67065250907247));
#11414=CARTESIAN_POINT('Ctrl Pts',(0.198480736990691,-0.0207054209301543,
1.68176722195424));
#11415=CARTESIAN_POINT('Ctrl Pts',(0.125027795368688,0.155535744436796,
1.69288193483602));
#11416=CARTESIAN_POINT('Ctrl Pts',(-0.0628819265359346,0.189391606802921,
1.7039966477178));
#11417=CARTESIAN_POINT('Ctrl Pts',(-0.193226346036818,0.0498687939449371,
1.71511136059957));
#11418=CARTESIAN_POINT('Ctrl Pts',(-0.146681575674501,-0.135306440238108,
1.72622607348135));
#11419=CARTESIAN_POINT('Ctrl Pts',(0.0341429428748287,-0.196615301703883,
1.73734078636313));
#11420=CARTESIAN_POINT('Ctrl Pts',(0.183711281153983,-0.0779325515367303,
1.7484554992449));
#11421=CARTESIAN_POINT('Ctrl Pts',(0.165101002186673,0.112093605924776,
1.75957021212668));
#11422=CARTESIAN_POINT('Ctrl Pts',(-0.00465110149246194,0.199503595624664,
1.77068492500845));
#11423=CARTESIAN_POINT('Ctrl Pts',(-0.170145351147817,0.104277883057956,
1.78179963789023));
#11424=CARTESIAN_POINT('Ctrl Pts',(-0.179879923404974,-0.0864090884576575,
1.79291435077201));
#11425=CARTESIAN_POINT('Ctrl Pts',(-0.0249432974721202,-0.197992801191054,
1.80402906365378));
#11426=CARTESIAN_POINT('Ctrl Pts',(0.152827687091721,-0.128323869449364,
1.81514377653556));
#11427=CARTESIAN_POINT('Ctrl Pts',(0.190692461592625,0.0588192358332533,
1.82625848941733));
#11428=CARTESIAN_POINT('Ctrl Pts',(0.0539876924676758,0.192116231678321,
1.83737320229911));
#11429=CARTESIAN_POINT('Ctrl Pts',(-0.132140146435612,0.149540292604495,
1.84848791518088));
#11430=CARTESIAN_POINT('Ctrl Pts',(-0.197300198436039,-0.0299324090136843,
1.85960262806266));
#11431=CARTESIAN_POINT('Ctrl Pts',(-0.0818416496243918,-0.182003466447815,
1.87071734094444));
#11432=CARTESIAN_POINT('Ctrl Pts',(0.108538892983941,-0.167459326769468,
1.88183205382621));
#11433=CARTESIAN_POINT('Ctrl Pts',(0.199557432209361,0.000385567463561441,
1.89294676670799));
#11434=CARTESIAN_POINT('Ctrl Pts',(0.107890984430119,0.167877493699908,
1.90406147958976));
#11435=CARTESIAN_POINT('Ctrl Pts',(-0.0825443384058951,0.18168585418077,
1.91517619247155));
#11436=CARTESIAN_POINT('Ctrl Pts',(-0.197414390522405,0.0291697759149795,
1.92629090535332));
#11437=CARTESIAN_POINT('Ctrl Pts',(-0.131561304603733,-0.150049793546099,
1.9374056182351));
#11438=CARTESIAN_POINT('Ctrl Pts',(0.0547296670692254,-0.191906177479399,
1.94852033111687));
#11439=CARTESIAN_POINT('Ctrl Pts',(0.190918327810351,-0.0580819207530336,
1.95963504399865));
#11440=CARTESIAN_POINT('Ctrl Pts',(0.152330675543031,0.128913469819363,
1.97074975688042));
#11441=CARTESIAN_POINT('Ctrl Pts',(-0.0257081972270486,0.19789493679121,
1.9818644697622));
#11442=CARTESIAN_POINT('Ctrl Pts',(-0.18021248336538,0.0857133493193614,
1.99297918264398));
#11443=CARTESIAN_POINT('Ctrl Pts',(-0.169741129071859,-0.104934582067508,
2.00409389552575));
#11444=CARTESIAN_POINT('Ctrl Pts',(-0.00388014275435722,-0.199520078950613,
2.01520860840753));
#11445=CARTESIAN_POINT('Ctrl Pts',(0.165532922885783,-0.111454783895257,
2.0263233212893));
#11446=CARTESIAN_POINT('Ctrl Pts',(0.183408761716666,0.0786418688605853,
2.03743803417108));
#11447=CARTESIAN_POINT('Ctrl Pts',(0.0333829249251954,0.196745769295354,
2.04855274705286));
#11448=CARTESIAN_POINT('Ctrl Pts',(-0.147203333186775,0.13473862145244,
2.05966745993463));
#11449=CARTESIAN_POINT('Ctrl Pts',(-0.193032199844087,-0.0506150890153994,
2.07078217281641));
#11450=CARTESIAN_POINT('Ctrl Pts',(-0.0621496078990471,-0.189633181826421,
2.08189688569819));
#11451=CARTESIAN_POINT('Ctrl Pts',(0.125627884849386,-0.155051449397732,
2.09301159857996));
#11452=CARTESIAN_POINT('Ctrl Pts',(0.19839924500399,0.0214722378164315,
2.10412631146174));
#11453=CARTESIAN_POINT('Ctrl Pts',(0.0895458813959111,0.178339150307365,
2.11524102434352));
#11454=CARTESIAN_POINT('Ctrl Pts',(-0.101282320179413,0.171945366415114,
2.12635573722529));
#11455=CARTESIAN_POINT('Ctrl Pts',(-0.199391552961908,0.00814407987298619,
2.13747045010707));
#11456=CARTESIAN_POINT('Ctrl Pts',(-0.114967652853453,-0.163112710028795,
2.14858516298884));
#11457=CARTESIAN_POINT('Ctrl Pts',(0.0747034629346199,-0.185047858812318,
2.15969987587062));
#11458=CARTESIAN_POINT('Ctrl Pts',(0.195987243349849,-0.0375808190699873,
2.17081458875239));
#11459=CARTESIAN_POINT('Ctrl Pts',(0.137854367504411,0.144289606370936,
2.18192930163417));
#11460=CARTESIAN_POINT('Ctrl Pts',(-0.0464773807617405,0.194070014828589,
2.19304401451595));
#11461=CARTESIAN_POINT('Ctrl Pts',(-0.188261383097489,0.0661888938220966,
2.20415872739772));
#11462=CARTESIAN_POINT('Ctrl Pts',(-0.157701366868572,-0.122284890412664,
2.2152734402795));
#11463=CARTESIAN_POINT('Ctrl Pts',(0.0172264588114365,-0.198812897372179,
2.22638815316128));
#11464=CARTESIAN_POINT('Ctrl Pts',(0.176384337838951,-0.0933374855090313,
2.23750286604305));
#11465=CARTESIAN_POINT('Ctrl Pts',(0.174071003916871,0.0975837590815798,
2.24861757892483));
#11466=CARTESIAN_POINT('Ctrl Pts',(0.0124043480086864,0.199171945650634,
2.25973229180661));
#11467=CARTESIAN_POINT('Ctrl Pts',(-0.160618061068349,0.118427923902816,
2.27084700468838));
#11468=CARTESIAN_POINT('Ctrl Pts',(-0.186602206238641,-0.0707308020764581,
2.28196171757016));
#11469=CARTESIAN_POINT('Ctrl Pts',(-0.0417619019469965,-0.195139384244164,
2.29307643045193));
#11470=CARTESIAN_POINT('Ctrl Pts',(0.141310632941521,-0.140906691078931,
2.30419114333371));
#11471=CARTESIAN_POINT('Ctrl Pts',(0.195017838673586,0.0423176190650909,
2.31530585621549));
#11472=CARTESIAN_POINT('Ctrl Pts',(0.0702004238379346,0.186805106982167,
2.32642056909726));
#11473=CARTESIAN_POINT('Ctrl Pts',(-0.118890753020677,0.160276271309004,
2.33753528197904));
#11474=CARTESIAN_POINT('Ctrl Pts',(-0.199126689652242,-0.0129671965109469,
2.34864999486081));
#11475=CARTESIAN_POINT('Ctrl Pts',(-0.0971035821632717,-0.174359600849589,
2.35976470774259));
#11476=CARTESIAN_POINT('Ctrl Pts',(0.0938732487360676,-0.176096776735865,
2.37087942062436));
#11477=CARTESIAN_POINT('Ctrl Pts',(0.198798975503885,-0.0166977068286914,
2.38199413350614));
#11478=CARTESIAN_POINT('Ctrl Pts',(0.121954858028878,0.158124624589868,
2.39310884638792));
#11479=CARTESIAN_POINT('Ctrl Pts',(-0.0669741409359997,0.187921788294323,
2.4042235592697));
#11480=CARTESIAN_POINT('Ctrl Pts',(-0.151381513586126,0.0934915980750552,
2.41163336785755));
#11481=CARTESIAN_POINT('Ctrl Pts',(-0.164302040955162,0.0388527191122167,
2.41533827215147));
#11482=CARTESIAN_POINT('Ctrl Pts',(0.0903606778650135,-0.126612599672289,
0.));
#11483=CARTESIAN_POINT('Ctrl Pts',(0.132465879166514,-0.0965630268723143,
0.0037049042939254));
#11484=CARTESIAN_POINT('Ctrl Pts',(0.183615222457176,0.00832016090824247,
0.0111147128817762));
#11485=CARTESIAN_POINT('Ctrl Pts',(0.0924018852348323,0.159092396164803,
0.0222294257635523));
#11486=CARTESIAN_POINT('Ctrl Pts',(-0.0834773491744035,0.163753054047276,
0.0333441386453285));
#11487=CARTESIAN_POINT('Ctrl Pts',(-0.182896947799478,0.0187420415954273,
0.0444588515271047));
#11488=CARTESIAN_POINT('Ctrl Pts',(-0.11490456949349,-0.143549243818714,
0.0555735644088809));
#11489=CARTESIAN_POINT('Ctrl Pts',(0.0582883981674798,-0.17436384297299,
0.0666882772906571));
#11490=CARTESIAN_POINT('Ctrl Pts',(0.178115364857574,-0.0455907972452466,
0.0778029901724332));
#11491=CARTESIAN_POINT('Ctrl Pts',(0.134889573452136,0.124936168947966,
0.0889177030542095));
#11492=CARTESIAN_POINT('Ctrl Pts',(-0.0318225855039178,0.181080880580275,
0.100032415935985));
#11493=CARTESIAN_POINT('Ctrl Pts',(-0.169401887523431,0.0714598939929528,
0.111147128817762));
#11494=CARTESIAN_POINT('Ctrl Pts',(-0.151902562935867,-0.103581685912858,
0.122261841699538));
#11495=CARTESIAN_POINT('Ctrl Pts',(0.00465630089802304,-0.183797982260963,
0.133376554581314));
#11496=CARTESIAN_POINT('Ctrl Pts',(0.156952427521129,-0.0957570050449602,
0.14449126746309));
#11497=CARTESIAN_POINT('Ctrl Pts',(0.165566412512777,0.0799451630251659,
0.155605980344867));
#11498=CARTESIAN_POINT('Ctrl Pts',(0.0226124784964766,0.182461279865869,
0.166720693226643));
#11499=CARTESIAN_POINT('Ctrl Pts',(-0.141042046410868,0.117943197747344,
0.177835406108419));
#11500=CARTESIAN_POINT('Ctrl Pts',(-0.175579543452357,-0.0545461194875494,
0.188950118990195));
#11501=CARTESIAN_POINT('Ctrl Pts',(-0.0493826231024586,-0.177101125876806,
0.200064831871971));
#11502=CARTESIAN_POINT('Ctrl Pts',(0.122021650540482,-0.137528801235027,
0.211179544753747));
#11503=CARTESIAN_POINT('Ctrl Pts',(0.181721122596515,0.027944365932959,
0.222294257635524));
#11504=CARTESIAN_POINT('Ctrl Pts',(0.0750638686912215,0.167835840141849,
0.2334089705173));
#11505=CARTESIAN_POINT('Ctrl Pts',(-0.100310654468725,0.154081882562785,
0.244523683399076));
#11506=CARTESIAN_POINT('Ctrl Pts',(-0.18385572098811,-0.000726440326955142,
0.255638396280852));
#11507=CARTESIAN_POINT('Ctrl Pts',(-0.0990899426121504,-0.154869742320406,
0.266753109162628));
#11508=CARTESIAN_POINT('Ctrl Pts',(0.0763877910491314,-0.167237433721381,
0.277867822044404));
#11509=CARTESIAN_POINT('Ctrl Pts',(0.181936269483671,-0.0265075025422269,
0.288982534926181));
#11510=CARTESIAN_POINT('Ctrl Pts',(0.120931066297065,0.138488739775033,
0.300097247807957));
#11511=CARTESIAN_POINT('Ctrl Pts',(-0.0507805637499992,0.17670537114635,
0.311211960689733));
#11512=CARTESIAN_POINT('Ctrl Pts',(-0.176005092188198,0.0531569503270556,
0.322326673571509));
#11513=CARTESIAN_POINT('Ctrl Pts',(-0.140105639306261,-0.119054036800316,
0.333441386453286));
#11514=CARTESIAN_POINT('Ctrl Pts',(0.0240536163419306,-0.182276924995041,
0.344556099335061));
#11515=CARTESIAN_POINT('Ctrl Pts',(0.166192972555312,-0.078634278260764,
0.355670812216838));
#11516=CARTESIAN_POINT('Ctrl Pts',(0.156190859040095,0.0969941719726652,
0.366785525098613));
#11517=CARTESIAN_POINT('Ctrl Pts',(0.00320371741518769,0.183829241523736,
0.37790023798039));
#11518=CARTESIAN_POINT('Ctrl Pts',(-0.152716269495902,0.102377706927133,
0.389014950862166));
#11519=CARTESIAN_POINT('Ctrl Pts',(-0.168832043657856,-0.0727955690871238,
0.400129663743942));
#11520=CARTESIAN_POINT('Ctrl Pts',(-0.030390408656302,-0.18132809188354,
0.411244376625719));
#11521=CARTESIAN_POINT('Ctrl Pts',(0.135872146613563,-0.123863689671489,
0.422359089507495));
#11522=CARTESIAN_POINT('Ctrl Pts',(0.177750452880091,0.0469918114711103,
0.433473802389271));
#11523=CARTESIAN_POINT('Ctrl Pts',(0.0569069861965436,0.174828626850531,
0.444588515271047));
#11524=CARTESIAN_POINT('Ctrl Pts',(-0.116032019694402,0.142618456905312,
0.455703228152823));
#11525=CARTESIAN_POINT('Ctrl Pts',(-0.182749434260409,-0.0201518763869515,
0.466817941034599));
#11526=CARTESIAN_POINT('Ctrl Pts',(-0.0821687549726806,-0.164474160738562,
0.477932653916376));
#11527=CARTESIAN_POINT('Ctrl Pts',(0.093633366925239,-0.158228462808239,
0.489047366798152));
#11528=CARTESIAN_POINT('Ctrl Pts',(0.183718759405662,-0.00713241101304534,
0.500162079679928));
#11529=CARTESIAN_POINT('Ctrl Pts',(0.105618688669037,0.150493011293707,
0.511276792561704));
#11530=CARTESIAN_POINT('Ctrl Pts',(-0.0691700824248357,0.170349504084268,
0.52239150544348));
#11531=CARTESIAN_POINT('Ctrl Pts',(-0.180637054530859,0.0342594275321448,
0.533506218325257));
#11532=CARTESIAN_POINT('Ctrl Pts',(-0.12673971224287,-0.133193465248897,
0.544620931207033));
#11533=CARTESIAN_POINT('Ctrl Pts',(0.0431815857942205,-0.178714309703255,
0.555735644088809));
#11534=CARTESIAN_POINT('Ctrl Pts',(0.173572271754774,-0.0606310178233981,
0.566850356970585));
#11535=CARTESIAN_POINT('Ctrl Pts',(0.145066103517367,0.112956980548805,
0.577965069852361));
#11536=CARTESIAN_POINT('Ctrl Pts',(-0.0162409278223676,0.183138434272774,
0.589079782734138));
#11537=CARTESIAN_POINT('Ctrl Pts',(-0.162680190744136,0.0856656838171876,
0.600194495615913));
#11538=CARTESIAN_POINT('Ctrl Pts',(-0.160193762435174,-0.0902297751370224,
0.61130920849769));
#11539=CARTESIAN_POINT('Ctrl Pts',(-0.0110578453815636,-0.183524325090524,
0.622423921379466));
#11540=CARTESIAN_POINT('Ctrl Pts',(0.148200983745356,-0.108811406852975,
0.633538634261242));
#11541=CARTESIAN_POINT('Ctrl Pts',(0.171789121533681,0.0655129877741882,
0.644653347143018));
#11542=CARTESIAN_POINT('Ctrl Pts',(0.0381127912063918,0.179863473198069,
0.655768060024794));
#11543=CARTESIAN_POINT('Ctrl Pts',(-0.130453919745491,0.129557819785036,
0.666882772906571));
#11544=CARTESIAN_POINT('Ctrl Pts',(-0.17959650116453,-0.0393516278427419,
0.677997485788347));
#11545=CARTESIAN_POINT('Ctrl Pts',(-0.0643273434762849,-0.172236601004835,
0.689112198670122));
#11546=CARTESIAN_POINT('Ctrl Pts',(0.10983032453655,-0.147447460665183,
0.7002269115519));
#11547=CARTESIAN_POINT('Ctrl Pts',(0.183443747273531,0.0123225577969614,
0.711341624433675));
#11548=CARTESIAN_POINT('Ctrl Pts',(0.0891234668368183,0.160811882345183,
0.722456337315452));
#11549=CARTESIAN_POINT('Ctrl Pts',(-0.0867849519149494,0.162085859856851,
0.733571050197227));
#11550=CARTESIAN_POINT('Ctrl Pts',(-0.183246027426955,0.0149782267526674,
0.744685763079004));
#11551=CARTESIAN_POINT('Ctrl Pts',(-0.111954402533252,-0.145841234216655,
0.75580047596078));
#11552=CARTESIAN_POINT('Ctrl Pts',(0.0618259562826469,-0.173150238157939,
0.766915188842555));
#11553=CARTESIAN_POINT('Ctrl Pts',(0.179007701381185,-0.0419487388444433,
0.778029901724333));
#11554=CARTESIAN_POINT('Ctrl Pts',(0.132316724534454,0.127654761967143,
0.789144614606108));
#11555=CARTESIAN_POINT('Ctrl Pts',(-0.0355036877557856,0.180396624137356,
0.800259327487885));
#11556=CARTESIAN_POINT('Ctrl Pts',(-0.170822224949343,0.0679942740807686,
0.81137404036966));
#11557=CARTESIAN_POINT('Ctrl Pts',(-0.149761440162857,-0.106653480415604,
0.822488753251438));
#11558=CARTESIAN_POINT('Ctrl Pts',(0.00839855685065273,-0.18366523374673,
0.833603466133212));
#11559=CARTESIAN_POINT('Ctrl Pts',(0.158870089284654,-0.0925405239616719,
0.844718179014991));
#11560=CARTESIAN_POINT('Ctrl Pts',(0.163903890459678,0.0833004714068091,
0.855832891896764));
#11561=CARTESIAN_POINT('Ctrl Pts',(0.0188917636673275,0.182883993585968,
0.866947604778543));
#11562=CARTESIAN_POINT('Ctrl Pts',(-0.143414841019688,0.115046239485315,
0.878062317660317));
#11563=CARTESIAN_POINT('Ctrl Pts',(-0.174432231980648,-0.0581106727775883,
0.889177030542094));
#11564=CARTESIAN_POINT('Ctrl Pts',(-0.0457655175701415,-0.178070130134034,
0.90029174342387));
#11565=CARTESIAN_POINT('Ctrl Pts',(0.124797271018106,-0.135015165780915,
0.911406456305646));
#11566=CARTESIAN_POINT('Ctrl Pts',(0.18111431299722,0.0316395238895826,
0.922521169187422));
#11567=CARTESIAN_POINT('Ctrl Pts',(0.071630133994783,0.169329789902144,
0.933635882069198));
#11568=CARTESIAN_POINT('Ctrl Pts',(-0.103427899877919,0.152006984613398,
0.944750594950975));
#11569=CARTESIAN_POINT('Ctrl Pts',(-0.183802792481824,-0.0044707180964717,
0.95586530783275));
#11570=CARTESIAN_POINT('Ctrl Pts',(-0.0959152937319705,-0.156855698885072,
0.966980020714528));
#11571=CARTESIAN_POINT('Ctrl Pts',(0.0797779258821927,-0.165647023475673,
0.978094733596302));
#11572=CARTESIAN_POINT('Ctrl Pts',(0.182438389002691,-0.0227966677941671,
0.989209446478081));
#11573=CARTESIAN_POINT('Ctrl Pts',(0.118085504862125,0.140922912920049,
1.00032415935986));
#11574=CARTESIAN_POINT('Ctrl Pts',(-0.0543688349964322,0.175634517181406,
1.01143887224163));
#11575=CARTESIAN_POINT('Ctrl Pts',(-0.177051187889545,0.0495613832667703,
1.02255358512341));
#11576=CARTESIAN_POINT('Ctrl Pts',(-0.137651910443638,-0.121882752658575,
1.03366829800518));
#11577=CARTESIAN_POINT('Ctrl Pts',(0.0277609020139879,-0.181749239788739,
1.04478301088696));
#11578=CARTESIAN_POINT('Ctrl Pts',(0.167759977846949,-0.0752332617743367,
1.05589772376874));
#11579=CARTESIAN_POINT('Ctrl Pts',(0.154183067891921,0.10015505688606,1.06701243665051));
#11580=CARTESIAN_POINT('Ctrl Pts',(-0.000540836401177662,0.183856360619919,
1.07812714953229));
#11581=CARTESIAN_POINT('Ctrl Pts',(-0.154769631643078,0.0992462340115768,
1.08924186241407));
#11582=CARTESIAN_POINT('Ctrl Pts',(-0.167314462362078,-0.0762189250049056,
1.10035657529584));
#11583=CARTESIAN_POINT('Ctrl Pts',(-0.0266911547466422,-0.181909417300769,
1.11147128817762));
#11584=CARTESIAN_POINT('Ctrl Pts',(0.138366588630194,-0.121070809839768,
1.12258600105939));
#11585=CARTESIAN_POINT('Ctrl Pts',(0.176756544363487,0.0506021528108583,
1.13370071394117));
#11586=CARTESIAN_POINT('Ctrl Pts',(0.053334601374032,0.175951340263971,
1.14481542682295));
#11587=CARTESIAN_POINT('Ctrl Pts',(-0.118912538708016,0.140225753634735,
1.15593013970472));
#11588=CARTESIAN_POINT('Ctrl Pts',(-0.182301114375512,-0.0238695945055889,
1.1670448525865));
#11589=CARTESIAN_POINT('Ctrl Pts',(-0.0788020109327346,-0.166113506125697,
1.17815956546827));
#11590=CARTESIAN_POINT('Ctrl Pts',(0.0968364469996555,-0.156288695614551,
1.18927427835005));
#11591=CARTESIAN_POINT('Ctrl Pts',(0.183825913682498,-0.00338929243493567,
1.20038899123183));
#11592=CARTESIAN_POINT('Ctrl Pts',(0.102531822692703,0.152612840808782,
1.2115037041136));
#11593=CARTESIAN_POINT('Ctrl Pts',(-0.0726250950973966,0.168905445165361,
1.22261841699538));
#11594=CARTESIAN_POINT('Ctrl Pts',(-0.181297320199323,0.0305734448984526,
1.23373312987716));
#11595=CARTESIAN_POINT('Ctrl Pts',(-0.124000790252096,-0.135747036289086,
1.24484784275893));
#11596=CARTESIAN_POINT('Ctrl Pts',(0.0468123474454561,-0.177797800804905,
1.25596255564071));
#11597=CARTESIAN_POINT('Ctrl Pts',(0.174771089844121,-0.0570834476806803,
1.26707726852248));
#11598=CARTESIAN_POINT('Ctrl Pts',(0.142735519209796,0.115887986436578,
1.27819198140426));
#11599=CARTESIAN_POINT('Ctrl Pts',(-0.0199673795378149,0.182769684572709,
1.28930669428604));
#11600=CARTESIAN_POINT('Ctrl Pts',(-0.164391127110762,0.082334750692938,
1.30042140716781));
#11601=CARTESIAN_POINT('Ctrl Pts',(-0.158322905592802,-0.0934735866920008,
1.31153612004959));
#11602=CARTESIAN_POINT('Ctrl Pts',(-0.00731787249863105,-0.183711465582603,
1.32265083293137));
#11603=CARTESIAN_POINT('Ctrl Pts',(0.150386311950183,-0.10577055839144,
1.33376554581314));
#11604=CARTESIAN_POINT('Ctrl Pts',(0.170419244869387,0.0689980783976093,
1.34488025869492));
#11605=CARTESIAN_POINT('Ctrl Pts',(0.0344417641967487,0.180602377402486,
1.35599497157669));
#11606=CARTESIAN_POINT('Ctrl Pts',(-0.133065452928399,0.126874107214099,
1.36710968445847));
#11607=CARTESIAN_POINT('Ctrl Pts',(-0.178757810692705,-0.0430011506911841,
1.37822439734024));
#11608=CARTESIAN_POINT('Ctrl Pts',(-0.0608062091124237,-0.173510975957692,
1.38933911022202));
#11609=CARTESIAN_POINT('Ctrl Pts',(0.112810477944863,-0.145180060305354,
1.4004538231038));
#11610=CARTESIAN_POINT('Ctrl Pts',(0.183154736262308,0.0160560402683587,
1.41156853598558));
#11611=CARTESIAN_POINT('Ctrl Pts',(0.0858298667327937,0.162593627861136,
1.42268324886735));
#11612=CARTESIAN_POINT('Ctrl Pts',(-0.0900680126570708,0.160284768273284,
1.43379796174913));
#11613=CARTESIAN_POINT('Ctrl Pts',(-0.183513068618488,0.0112431085844059,
1.44491267463091));
#11614=CARTESIAN_POINT('Ctrl Pts',(-0.108960961133834,-0.148091062502792,
1.45602738751268));
#11615=CARTESIAN_POINT('Ctrl Pts',(0.0653395323085358,-0.171855169727642,
1.46714210039446));
#11616=CARTESIAN_POINT('Ctrl Pts',(0.179824906471596,-0.0382943449728064,
1.47825681327623));
#11617=CARTESIAN_POINT('Ctrl Pts',(0.129689447733715,0.130323063925534,
1.48937152615801));
#11618=CARTESIAN_POINT('Ctrl Pts',(-0.0391703041140288,0.179636135340385,
1.50048623903978));
#11619=CARTESIAN_POINT('Ctrl Pts',(-0.172171574426829,0.0645011845147166,
1.51160095192156));
#11620=CARTESIAN_POINT('Ctrl Pts',(-0.147558259862935,-0.109681419532377,
1.52271566480334));
#11621=CARTESIAN_POINT('Ctrl Pts',(0.0121373640243727,-0.183456093490935,
1.53383037768511));
#11622=CARTESIAN_POINT('Ctrl Pts',(0.160721829762796,-0.0892857619226799,
1.54494509056689));
#11623=CARTESIAN_POINT('Ctrl Pts',(0.162173387162441,0.0866212811073344,
1.55605980344866));
#11624=CARTESIAN_POINT('Ctrl Pts',(0.0151632070148183,0.183230813449705,
1.56717451633044));
#11625=CARTESIAN_POINT('Ctrl Pts',(-0.145728141304706,0.112101573032185,
1.57828922921222));
#11626=CARTESIAN_POINT('Ctrl Pts',(-0.173212563579333,-0.0616511286408472,
1.58940394209399));
#11627=CARTESIAN_POINT('Ctrl Pts',(-0.042129426749787,-0.178965262680077,
1.60051865497577));
#11628=CARTESIAN_POINT('Ctrl Pts',(0.127521122443655,-0.132445525311824,
1.61163336785754));
#11629=CARTESIAN_POINT('Ctrl Pts',(0.180432373388368,0.0353215582591597,
1.62274808073932));
#11630=CARTESIAN_POINT('Ctrl Pts',(0.0681666854301347,0.170753497304986,
1.6338627936211));
#11631=CARTESIAN_POINT('Ctrl Pts',(-0.106502241054892,0.149869031139527,
1.64497750650287));
#11632=CARTESIAN_POINT('Ctrl Pts',(-0.183673618550271,-0.00821314148570485,
1.65609221938465));
#11633=CARTESIAN_POINT('Ctrl Pts',(-0.0927008570553628,-0.158776588153342,
1.66720693226643));
#11634=CARTESIAN_POINT('Ctrl Pts',(0.0831349670626055,-0.163987899236237,
1.6783216451482));
#11635=CARTESIAN_POINT('Ctrl Pts',(0.182864829055688,-0.0190763764601355,
1.68943635802998));
#11636=CARTESIAN_POINT('Ctrl Pts',(0.115190958951233,0.143298628117334,
1.70055107091176));
#11637=CARTESIAN_POINT('Ctrl Pts',(-0.0579345528489473,0.174490806149227,
1.71166578379353));
#11638=CARTESIAN_POINT('Ctrl Pts',(-0.178023838851097,0.0459452570472002,
1.72278049667531));
#11639=CARTESIAN_POINT('Ctrl Pts',(-0.135141080530122,-0.124660908859055,
1.73389520955708));
#11640=CARTESIAN_POINT('Ctrl Pts',(0.0314566718510104,-0.181146160987399,
1.74500992243886));
#11641=CARTESIAN_POINT('Ctrl Pts',(0.169257392597246,-0.071801036869925,
1.75612463532064));
#11642=CARTESIAN_POINT('Ctrl Pts',(0.15211131820417,0.103274395271066,1.76723934820241));
#11643=CARTESIAN_POINT('Ctrl Pts',(-0.00428516586664415,0.18380721203998,
1.77835406108419));
#11644=CARTESIAN_POINT('Ctrl Pts',(-0.156758791931151,0.0960735915676151,
1.78946877396597));
#11645=CARTESIAN_POINT('Ctrl Pts',(-0.165727475334516,-0.0796106636303336,
1.80058348684774));
#11646=CARTESIAN_POINT('Ctrl Pts',(-0.0229808287568944,-0.182415282676811,
1.81169819972952));
#11647=CARTESIAN_POINT('Ctrl Pts',(0.140803633131985,-0.118227707163963,
1.82281291261129));
#11648=CARTESIAN_POINT('Ctrl Pts',(0.175689313331093,0.0541915032607811,
1.83392762549307));
#11649=CARTESIAN_POINT('Ctrl Pts',(0.0497400921817236,0.177001065178062,
1.84504233837485));
#11650=CARTESIAN_POINT('Ctrl Pts',(-0.121743730176064,0.137774881626631,
1.85615705125662));
#11651=CARTESIAN_POINT('Ctrl Pts',(-0.181777171964813,-0.0275774109896026,
1.8672717641384));
#11652=CARTESIAN_POINT('Ctrl Pts',(-0.0754025780794165,-0.16768394396421,
1.87838647702017));
#11653=CARTESIAN_POINT('Ctrl Pts',(0.0999993571785868,-0.154284096420481,
1.88950118990195));
#11654=CARTESIAN_POINT('Ctrl Pts',(0.183856812913126,0.000355232096483363,
1.90061590278373));
#11655=CARTESIAN_POINT('Ctrl Pts',(0.0994024242533403,0.154669363149183,
1.9117306156655));
#11656=CARTESIAN_POINT('Ctrl Pts',(-0.0760499812776094,0.167391320539895,
1.92284532854728));
#11657=CARTESIAN_POINT('Ctrl Pts',(-0.181882379737966,0.0268747797250293,
1.93396004142905));
#11658=CARTESIAN_POINT('Ctrl Pts',(-0.121210429996709,-0.138244296462558,
1.94507475431083));
#11659=CARTESIAN_POINT('Ctrl Pts',(0.050423690301781,-0.176807537454614,
1.95618946719261));
#11660=CARTESIAN_POINT('Ctrl Pts',(0.175897409028035,-0.0535121980639788,
1.96730418007439));
#11661=CARTESIAN_POINT('Ctrl Pts',(0.140345725058553,0.118770919429821,
1.97841889295616));
#11662=CARTESIAN_POINT('Ctrl Pts',(-0.0236855483435345,0.18232511797358,
1.98953360583794));
#11663=CARTESIAN_POINT('Ctrl Pts',(-0.166033870409582,0.0789696632969042,
2.00064831871971));
#11664=CARTESIAN_POINT('Ctrl Pts',(-0.156386372914875,-0.0966786233401791,
2.01176303160149));
#11665=CARTESIAN_POINT('Ctrl Pts',(-0.00357486400063734,-0.183822398504055,
2.02287774448326));
#11666=CARTESIAN_POINT('Ctrl Pts',(0.152509256593582,-0.102685833967865,
2.03399245736504));
#11667=CARTESIAN_POINT('Ctrl Pts',(0.168978674541131,0.072454547095341,
2.04510717024682));
#11668=CARTESIAN_POINT('Ctrl Pts',(0.0307564499829109,0.181266363754544,
2.05622188312859));
#11669=CARTESIAN_POINT('Ctrl Pts',(-0.135621787624101,0.124137764463539,
2.06733659601037));
#11670=CARTESIAN_POINT('Ctrl Pts',(-0.177844967536513,-0.046632835713789,
2.07845130889214));
#11671=CARTESIAN_POINT('Ctrl Pts',(-0.0572598509893232,-0.174713374727145,
2.08956602177392));
#11672=CARTESIAN_POINT('Ctrl Pts',(0.115743835073967,-0.142852436054201,
2.10068073465569));
#11673=CARTESIAN_POINT('Ctrl Pts',(0.182789748630034,0.0197828623436046,
2.11179544753748));
#11674=CARTESIAN_POINT('Ctrl Pts',(0.0825006624943804,0.164307925944582,
2.12291016041925));
#11675=CARTESIAN_POINT('Ctrl Pts',(-0.0933137111781269,0.15841718704366,
2.13402487330103));
#11676=CARTESIAN_POINT('Ctrl Pts',(-0.183703984579811,0.00750332650094965,
2.1451395861828));
#11677=CARTESIAN_POINT('Ctrl Pts',(-0.105922320244947,-0.150279459298985,
2.15625429906458));
#11678=CARTESIAN_POINT('Ctrl Pts',(0.0688260039060977,-0.170488812072594,
2.16736901194635));
#11679=CARTESIAN_POINT('Ctrl Pts',(0.180567516503863,-0.0346240655854127,
2.17848372482813));
#11680=CARTESIAN_POINT('Ctrl Pts',(0.127008372351303,0.132937304665343,
2.18959843770991));
#11681=CARTESIAN_POINT('Ctrl Pts',(-0.0428206707452402,0.178801130147604,
2.20071315059168));
#11682=CARTESIAN_POINT('Ctrl Pts',(-0.173449505276293,0.0609813372203028,
2.21182786347346));
#11683=CARTESIAN_POINT('Ctrl Pts',(-0.145293865447621,-0.112663858067262,
2.22294257635523));
#11684=CARTESIAN_POINT('Ctrl Pts',(0.0158711293274525,-0.18317085598959,
2.23405728923701));
#11685=CARTESIAN_POINT('Ctrl Pts',(0.162506912640762,-0.0859939538258468,
2.24517200211879));
#11686=CARTESIAN_POINT('Ctrl Pts',(0.160375585346118,0.0899061424983564,
2.25628671500056));
#11687=CARTESIAN_POINT('Ctrl Pts',(0.011428408683624,0.183501655356106,
2.26740142788234));
#11688=CARTESIAN_POINT('Ctrl Pts',(-0.147981082324864,0.109110346869202,
2.27851614076412));
#11689=CARTESIAN_POINT('Ctrl Pts',(-0.171920867801111,-0.0651659008666877,
2.28963085364589));
#11690=CARTESIAN_POINT('Ctrl Pts',(-0.0384761925835495,-0.179786364575594,
2.30074556652767));
#11691=CARTESIAN_POINT('Ctrl Pts',(0.130192708513641,-0.129820547664333,
2.31186027940944));
#11692=CARTESIAN_POINT('Ctrl Pts',(0.179674381869752,0.0389881874367674,
2.32297499229122));
#11693=CARTESIAN_POINT('Ctrl Pts',(0.0646772513010348,0.172107804882976,
2.33408970517299));
#11694=CARTESIAN_POINT('Ctrl Pts',(-0.109536761889629,0.147666183625563,
2.34520441805478));
#11695=CARTESIAN_POINT('Ctrl Pts',(-0.183459959972792,-0.0119469738436946,
2.35631913093654));
#11696=CARTESIAN_POINT('Ctrl Pts',(-0.0894637445537859,-0.160641476281263,
2.36743384381833));
#11697=CARTESIAN_POINT('Ctrl Pts',(0.0864875647042136,-0.162241976039076,
2.3785485567001));
#11698=CARTESIAN_POINT('Ctrl Pts',(0.183158029454863,-0.0153839780683336,
2.38966326958188));
#11699=CARTESIAN_POINT('Ctrl Pts',(0.112359791706175,0.145683822438027,
2.40077798246366));
#11700=CARTESIAN_POINT('Ctrl Pts',(-0.0617048032927588,0.173136628840171,
2.41189269534543));
#11701=CARTESIAN_POINT('Ctrl Pts',(-0.139471240503386,0.0861359412472379,
2.41930250393328));
#11702=CARTESIAN_POINT('Ctrl Pts',(-0.15137521700242,0.0357958960981592,
2.42300740822721));
#11703=CARTESIAN_POINT('Ctrl Pts',(0.103461767481305,0.116497970106856,
2.4));
#11704=CARTESIAN_POINT('Ctrl Pts',(0.101062838412544,0.119258880418799,
2.4));
#11705=CARTESIAN_POINT('Ctrl Pts',(0.0985654514169239,0.121922998634947,
2.4));
#11706=CARTESIAN_POINT('Ctrl Pts',(0.0959729906474675,0.124483778490476,
2.4));
#11707=CARTESIAN_POINT('Ctrl Pts',(0.0883686915733725,0.131995149969571,
2.4));
#11708=CARTESIAN_POINT('Ctrl Pts',(0.0799499756415848,0.138619651568493,
2.4));
#11709=CARTESIAN_POINT('Ctrl Pts',(0.0709074190314827,0.144354628951697,
2.4));
#11710=CARTESIAN_POINT('Ctrl Pts',(0.0663081210711623,0.147271599330582,
2.4));
#11711=CARTESIAN_POINT('Ctrl Pts',(0.0615466559749117,0.149958011111103,
2.4));
#11712=CARTESIAN_POINT('Ctrl Pts',(0.0566442332600693,0.152410331606476,
2.4));
#11713=CARTESIAN_POINT('Ctrl Pts',(0.0538846120488591,0.153790766556572,
2.4));
#11714=CARTESIAN_POINT('Ctrl Pts',(0.0510823344409583,0.155095773985438,
2.4));
#11715=CARTESIAN_POINT('Ctrl Pts',(0.0482496499195413,0.156321567055163,
2.4));
#11716=CARTESIAN_POINT('Ctrl Pts',(0.0376888807059046,0.160891549209958,
2.4));
#11717=CARTESIAN_POINT('Ctrl Pts',(0.026677561630956,0.164379337372229,
2.4));
#11718=CARTESIAN_POINT('Ctrl Pts',(0.0154207238187948,0.166770147581746,
2.4));
#11719=CARTESIAN_POINT('Ctrl Pts',(0.00969748088526884,0.167985692112577,
2.4));
#11720=CARTESIAN_POINT('Ctrl Pts',(0.00391012467736534,0.168917061289908,
2.4));
#11721=CARTESIAN_POINT('Ctrl Pts',(-0.00191715667191961,0.169557978194554,
2.4));
#11722=CARTESIAN_POINT('Ctrl Pts',(-0.00616200194240661,0.170024849953164,
2.4));
#11723=CARTESIAN_POINT('Ctrl Pts',(-0.0104304763189531,0.170337222982092,
2.4));
#11724=CARTESIAN_POINT('Ctrl Pts',(-0.0146899072891042,0.170491883891854,
2.4));
#11725=CARTESIAN_POINT('Ctrl Pts',(-0.0266165983220355,0.170924944762785,
2.4));
#11726=CARTESIAN_POINT('Ctrl Pts',(-0.0385088145683558,0.170130732075648,
2.4));
#11727=CARTESIAN_POINT('Ctrl Pts',(-0.0501623159300862,0.168075457674568,
2.4));
#11728=CARTESIAN_POINT('Ctrl Pts',(-0.0531380387349214,0.167550643138949,
2.4));
#11729=CARTESIAN_POINT('Ctrl Pts',(-0.056098276264386,0.166943351080139,
2.4));
#11730=CARTESIAN_POINT('Ctrl Pts',(-0.0590397244743148,0.166252475819097,
2.4));
#11731=CARTESIAN_POINT('Ctrl Pts',(-0.0636086044060329,0.165179356086839,
2.4));
#11732=CARTESIAN_POINT('Ctrl Pts',(-0.0681321698191967,0.163904647115538,
2.4));
#11733=CARTESIAN_POINT('Ctrl Pts',(-0.0726033638424945,0.16243676026702,
2.4));
#11734=CARTESIAN_POINT('Ctrl Pts',(-0.0761928889181732,0.161258324121428,
2.4));
#11735=CARTESIAN_POINT('Ctrl Pts',(-0.0797406633513067,0.159957854461999,
2.4));
#11736=CARTESIAN_POINT('Ctrl Pts',(-0.0832382631684214,0.158543149031954,
2.4));
#11737=CARTESIAN_POINT('Ctrl Pts',(-0.0942712060188925,0.154080556117935,
2.4));
#11738=CARTESIAN_POINT('Ctrl Pts',(-0.104821070590689,0.148480110064895,
2.4));
#11739=CARTESIAN_POINT('Ctrl Pts',(-0.114778874587596,0.14189890553014,
2.4));
#11740=CARTESIAN_POINT('Ctrl Pts',(-0.119667974430172,0.13866765433612,
2.4));
#11741=CARTESIAN_POINT('Ctrl Pts',(-0.124414280597228,0.135199161922686,
2.4));
#11742=CARTESIAN_POINT('Ctrl Pts',(-0.129003727534357,0.131507805861248,
2.4));
#11743=CARTESIAN_POINT('Ctrl Pts',(-0.132789110117922,0.128463169952799,
2.4));
#11744=CARTESIAN_POINT('Ctrl Pts',(-0.136469556648549,0.125264639778438,
2.4));
#11745=CARTESIAN_POINT('Ctrl Pts',(-0.140019314144638,0.121936802656766,
2.4));
#11746=CARTESIAN_POINT('Ctrl Pts',(-0.146223653031234,0.116120340747751,
2.4));
#11747=CARTESIAN_POINT('Ctrl Pts',(-0.152041126912371,0.109900559216443,
2.4));
#11748=CARTESIAN_POINT('Ctrl Pts',(-0.157432164500961,0.103324206966413,
2.4));
#11749=CARTESIAN_POINT('Ctrl Pts',(-0.160741343411017,0.0992874467299484,
2.4));
#11750=CARTESIAN_POINT('Ctrl Pts',(-0.163889774361174,0.0951161328995282,
2.4));
#11751=CARTESIAN_POINT('Ctrl Pts',(-0.166867208569052,0.0908194395900732,
2.4));
#11752=CARTESIAN_POINT('Ctrl Pts',(-0.16945817546063,0.0870804518137491,
2.4));
#11753=CARTESIAN_POINT('Ctrl Pts',(-0.171914118235205,0.0832543718370342,
2.4));
#11754=CARTESIAN_POINT('Ctrl Pts',(-0.17422826794027,0.0793498140525304,
2.4));
#11755=CARTESIAN_POINT('Ctrl Pts',(-0.180683508174901,0.0684581857132719,
2.4));
#11756=CARTESIAN_POINT('Ctrl Pts',(-0.186040971013606,0.0569542137720182,
2.4));
#11757=CARTESIAN_POINT('Ctrl Pts',(-0.190155688860645,0.0449663651403318,
2.4));
#11758=CARTESIAN_POINT('Ctrl Pts',(0.0863566694936597,0.175642871684081,
0.));
#11759=CARTESIAN_POINT('Ctrl Pts',(0.0902251377602554,0.173267020623209,
-1.48058408815148E-18));
#11760=CARTESIAN_POINT('Ctrl Pts',(0.0939991325874577,0.170750246590702,
-3.18714891677109E-17));
#11761=CARTESIAN_POINT('Ctrl Pts',(0.0976698484646397,0.168092084222829,
-2.37440275774325E-17));
#11762=CARTESIAN_POINT('Ctrl Pts',(0.104809934079732,0.162921565032443,
-6.47830459115438E-18));
#11763=CARTESIAN_POINT('Ctrl Pts',(0.11155987158375,0.157216438110753,-1.30821889653785E-17));
#11764=CARTESIAN_POINT('Ctrl Pts',(0.117888926389013,0.151039119528356,
-2.51534904016637E-17));
#11765=CARTESIAN_POINT('Ctrl Pts',(0.12275959422371,0.146285223749331,-3.4443234516339E-17));
#11766=CARTESIAN_POINT('Ctrl Pts',(0.127384674495468,0.141245910799109,
-5.49491509124901E-17));
#11767=CARTESIAN_POINT('Ctrl Pts',(0.131724318639059,0.135976688450155,
-4.46691295064028E-17));
#11768=CARTESIAN_POINT('Ctrl Pts',(0.13624098258323,0.130492527581232,-3.39697724868313E-17));
#11769=CARTESIAN_POINT('Ctrl Pts',(0.140453276997769,0.124755769602575,
2.19954579643677E-17));
#11770=CARTESIAN_POINT('Ctrl Pts',(0.144343923096435,0.11879886899313,2.34187669256869E-17));
#11771=CARTESIAN_POINT('Ctrl Pts',(0.14782723598055,0.113465629187694,2.46930618158692E-17));
#11772=CARTESIAN_POINT('Ctrl Pts',(0.151052683365278,0.107955843865382,
-2.41963381637405E-17));
#11773=CARTESIAN_POINT('Ctrl Pts',(0.154004429688849,0.102292097260694,
-2.77555756156289E-17));
#11774=CARTESIAN_POINT('Ctrl Pts',(0.155739361180546,0.098963148472989,
-2.98475687833339E-17));
#11775=CARTESIAN_POINT('Ctrl Pts',(0.157375218128347,0.0955895675179438,
-1.47300813205832E-17));
#11776=CARTESIAN_POINT('Ctrl Pts',(0.158909878065559,0.0921763188170318,
-1.38777878078145E-17));
#11777=CARTESIAN_POINT('Ctrl Pts',(0.163914736043458,0.0810449765716888,
-1.10982743250791E-17));
#11778=CARTESIAN_POINT('Ctrl Pts',(0.167847252202745,0.0694917728439882,
9.78508137823812E-19));
#11779=CARTESIAN_POINT('Ctrl Pts',(0.170602677001,0.0576812257767674,-6.93889390390723E-18));
#11780=CARTESIAN_POINT('Ctrl Pts',(0.171991086671603,0.051730100645855,
-1.0928332326523E-17));
#11781=CARTESIAN_POINT('Ctrl Pts',(0.173079837921644,0.045713571791822,
2.82966050020454E-17));
#11782=CARTESIAN_POINT('Ctrl Pts',(0.173850319068363,0.0396534029415724,
3.12250225675825E-17));
#11783=CARTESIAN_POINT('Ctrl Pts',(0.174328221535971,0.0358944924737595,
3.30414174095796E-17));
#11784=CARTESIAN_POINT('Ctrl Pts',(0.17468335594369,0.0321178316076463,
1.10401303661207E-17));
#11785=CARTESIAN_POINT('Ctrl Pts',(0.174910473855443,0.0283454744478527,
1.04083408558608E-17));
#11786=CARTESIAN_POINT('Ctrl Pts',(0.175316978609887,0.0215935581895444,
9.277538631825E-18));
#11787=CARTESIAN_POINT('Ctrl Pts',(0.175315699739124,0.0148427717406492,
1.46103290560722E-17));
#11788=CARTESIAN_POINT('Ctrl Pts',(0.174886275518905,0.00812263339345144,
8.67361737988404E-18));
#11789=CARTESIAN_POINT('Ctrl Pts',(0.174132950249562,-0.00366629185126618,
-1.74096734056434E-18));
#11790=CARTESIAN_POINT('Ctrl Pts',(0.172064162512452,-0.015362891267024,
2.05614309001684E-17));
#11791=CARTESIAN_POINT('Ctrl Pts',(0.168769206728486,-0.0267893073475998,
3.29597460435593E-17));
#11792=CARTESIAN_POINT('Ctrl Pts',(0.16774389460927,-0.0303449371207288,
3.68178077620904E-17));
#11793=CARTESIAN_POINT('Ctrl Pts',(0.166598934891851,-0.0338750081296103,
-1.14228928110452E-17));
#11794=CARTESIAN_POINT('Ctrl Pts',(0.165342739336206,-0.0373581457979936,
-1.21430643318376E-17));
#11795=CARTESIAN_POINT('Ctrl Pts',(0.161971436695734,-0.0467059827377018,
-1.40758176668829E-17));
#11796=CARTESIAN_POINT('Ctrl Pts',(0.15779349911764,-0.0557446055141624,
4.46068520704283E-18));
#11797=CARTESIAN_POINT('Ctrl Pts',(0.152869055079828,-0.0643699094100016,
3.46944695195361E-17));
#11798=CARTESIAN_POINT('Ctrl Pts',(0.150138152047912,-0.0691531637996316,
5.14609374926382E-17));
#11799=CARTESIAN_POINT('Ctrl Pts',(0.147177244350092,-0.0738090201013192,
-1.50318967518465E-18));
#11800=CARTESIAN_POINT('Ctrl Pts',(0.143994070896324,-0.0783167975121378,
-6.93889390390723E-18));
#11801=CARTESIAN_POINT('Ctrl Pts',(0.14200814232103,-0.0811291242989852,
-1.03301386825709E-17));
#11802=CARTESIAN_POINT('Ctrl Pts',(0.139935669748527,-0.0838837680603148,
1.78075490207948E-17));
#11803=CARTESIAN_POINT('Ctrl Pts',(0.137778285309418,-0.0865751700254918,
2.08166817117217E-17));
#11804=CARTESIAN_POINT('Ctrl Pts',(0.135528080086737,-0.0893823687095031,
2.39552813855276E-17));
#11805=CARTESIAN_POINT('Ctrl Pts',(0.133190359351591,-0.0921145253789638,
2.01371011364845E-17));
#11806=CARTESIAN_POINT('Ctrl Pts',(0.130771621045583,-0.0947623052516935,
1.73472347597681E-17));
#11807=CARTESIAN_POINT('Ctrl Pts',(0.123528051428705,-0.102691802126427,
8.99222120938157E-18));
#11808=CARTESIAN_POINT('Ctrl Pts',(0.11554930715408,-0.109880506845132,
-2.43949043573933E-17));
#11809=CARTESIAN_POINT('Ctrl Pts',(0.106897890251738,-0.116170853237509,
-6.93889390390723E-18));
#11810=CARTESIAN_POINT('Ctrl Pts',(0.101631397195622,-0.120000060172047,
3.68733748437521E-18));
#11811=CARTESIAN_POINT('Ctrl Pts',(0.0961151553280942,-0.12349557915736,
2.54302973394793E-18));
#11812=CARTESIAN_POINT('Ctrl Pts',(0.0903606778650135,-0.126612599672289,
0.));
#11813=CARTESIAN_POINT('Origin',(0.,0.,0.));
#11814=CARTESIAN_POINT('Origin',(0.,0.,2.4));
#11815=CARTESIAN_POINT('Origin',(-0.0866025403784439,-0.15,-0.3));
#11816=CARTESIAN_POINT('',(-0.0866025403784439,-0.15,-0.3));
#11817=CARTESIAN_POINT('',(0.0866025403784439,-0.15,-0.3));
#11818=CARTESIAN_POINT('',(-0.043301270189222,-0.15,-0.3));
#11819=CARTESIAN_POINT('',(-0.0866025403784439,-0.15,-0.1));
#11820=CARTESIAN_POINT('',(-0.0866025403784439,-0.15,-0.3));
#11821=CARTESIAN_POINT('',(0.0866025403784439,-0.15,-0.1));
#11822=CARTESIAN_POINT('',(-0.0866025403784439,-0.15,-0.1));
#11823=CARTESIAN_POINT('',(0.0866025403784439,-0.15,-0.3));
#11824=CARTESIAN_POINT('Origin',(-0.173205080756888,2.12115047744981E-17,
-0.3));
#11825=CARTESIAN_POINT('',(-0.173205080756888,2.12115047744981E-17,-0.3));
#11826=CARTESIAN_POINT('',(-0.151554445662277,-0.0375,-0.3));
#11827=CARTESIAN_POINT('',(-0.173205080756888,2.77555756156289E-17,-0.1));
#11828=CARTESIAN_POINT('',(-0.173205080756888,2.12115047744981E-17,-0.3));
#11829=CARTESIAN_POINT('',(-0.173205080756888,2.12115047744981E-17,-0.1));
#11830=CARTESIAN_POINT('Origin',(-0.0866025403784438,0.15,-0.3));
#11831=CARTESIAN_POINT('',(-0.0866025403784438,0.15,-0.3));
#11832=CARTESIAN_POINT('',(-0.108253175473055,0.1125,-0.3));
#11833=CARTESIAN_POINT('',(-0.0866025403784438,0.15,-0.1));
#11834=CARTESIAN_POINT('',(-0.0866025403784438,0.15,-0.3));
#11835=CARTESIAN_POINT('',(-0.0866025403784438,0.15,-0.1));
#11836=CARTESIAN_POINT('Origin',(0.0866025403784439,0.15,-0.3));
#11837=CARTESIAN_POINT('',(0.0866025403784439,0.15,-0.3));
#11838=CARTESIAN_POINT('',(0.043301270189222,0.15,-0.3));
#11839=CARTESIAN_POINT('',(0.0866025403784439,0.15,-0.1));
#11840=CARTESIAN_POINT('',(0.0866025403784439,0.15,-0.3));
#11841=CARTESIAN_POINT('',(0.0866025403784439,0.15,-0.1));
#11842=CARTESIAN_POINT('Origin',(0.173205080756888,0.,-0.3));
#11843=CARTESIAN_POINT('',(0.173205080756888,0.,-0.3));
#11844=CARTESIAN_POINT('',(0.151554445662277,0.0375,-0.3));
#11845=CARTESIAN_POINT('',(0.173205080756888,0.,-0.1));
#11846=CARTESIAN_POINT('',(0.173205080756888,0.,-0.3));
#11847=CARTESIAN_POINT('',(0.173205080756888,0.,-0.1));
#11848=CARTESIAN_POINT('Origin',(0.0866025403784439,-0.15,-0.3));
#11849=CARTESIAN_POINT('',(0.108253175473055,-0.1125,-0.3));
#11850=CARTESIAN_POINT('',(0.0866025403784439,-0.15,-0.1));
#11851=CARTESIAN_POINT('Origin',(0.,2.77555756156289E-17,-0.1));
#11852=CARTESIAN_POINT('Origin',(0.,0.,0.));
#11853=CARTESIAN_POINT('',(-0.4,-4.89858719658941E-17,0.));
#11854=CARTESIAN_POINT('Origin',(0.,0.,0.));
#11855=CARTESIAN_POINT('Origin',(0.,0.,-0.3));
#11856=CARTESIAN_POINT('',(-0.4,-4.89858719658941E-17,-0.3));
#11857=CARTESIAN_POINT('',(-0.4,-4.89858719658941E-17,-0.3));
#11858=CARTESIAN_POINT('Origin',(0.,0.,-0.3));
#11859=CARTESIAN_POINT('Origin',(0.,0.,-0.3));
#11860=CARTESIAN_POINT('Origin',(0.,0.,2.4));
#11861=CARTESIAN_POINT('',(0.,0.,0.));
#11862=CARTESIAN_POINT('Origin',(0.,0.,0.2));
#11863=CARTESIAN_POINT('',(-0.166448982935848,-0.000123056367485261,0.00714803633902118));
#11864=CARTESIAN_POINT('',(-0.1666,2.04026156737949E-17,0.));
#11865=CARTESIAN_POINT('',(-0.1666,2.04026156737949E-17,0.2));
#11866=CARTESIAN_POINT('',(-0.133707694182663,0.0998962258211753,-3.72972504691399E-17));
#11867=CARTESIAN_POINT('Origin',(0.,0.,0.));
#11868=CARTESIAN_POINT('Ctrl Pts',(-0.13370774202371,0.0998962637199352,
-7.80625564189563E-17));
#11869=CARTESIAN_POINT('Ctrl Pts',(-0.154908007636265,0.0714511367790156,
0.00238267877967367));
#11870=CARTESIAN_POINT('Ctrl Pts',(-0.166218419498132,0.0355914785578886,
0.00476535755934742));
#11871=CARTESIAN_POINT('Ctrl Pts',(-0.166448982935848,-0.000123056367485261,
0.00714803633902118));
#11872=CARTESIAN_POINT('Origin',(0.,0.,0.2));
#11873=CARTESIAN_POINT('',(-0.166860410748999,-4.21553466717637E-5,0.0771480363390211));
#11874=CARTESIAN_POINT('',(-0.166654775959782,0.000146646548331295,0.0578519636609792));
#11875=CARTESIAN_POINT('',(-0.1666,2.04026156737949E-17,0.2));
#11876=CARTESIAN_POINT('',(-0.0769902040670466,-0.147743251885541,0.));
#11877=CARTESIAN_POINT('Ctrl Pts',(-0.166654775959782,0.000146646548331295,
0.0578519636609792));
#11878=CARTESIAN_POINT('Ctrl Pts',(-0.166758996638221,0.0114358133562754,
0.0570962429544575));
#11879=CARTESIAN_POINT('Ctrl Pts',(-0.165709525805481,0.0227058575110541,
0.0563405222479359));
#11880=CARTESIAN_POINT('Ctrl Pts',(-0.163435150898545,0.0337234259760408,
0.0555848015414142));
#11881=CARTESIAN_POINT('Ctrl Pts',(-0.15228282290737,0.0877477369249823,
0.0518791481053199));
#11882=CARTESIAN_POINT('Ctrl Pts',(-0.11167888524593,0.1357015190679,0.0481734946692255));
#11883=CARTESIAN_POINT('Ctrl Pts',(-0.0602476828221599,0.15561740130089,
0.0444678412331313));
#11884=CARTESIAN_POINT('Ctrl Pts',(-0.00881648039838925,0.175533283533879,
0.040762187797037));
#11885=CARTESIAN_POINT('Ctrl Pts',(0.053441986787712,0.16741126585694,0.0370565343609427));
#11886=CARTESIAN_POINT('Ctrl Pts',(0.0980813920646122,0.134988882613172,
0.0333508809248484));
#11887=CARTESIAN_POINT('Ctrl Pts',(0.142720797341511,0.102566499369405,
0.0296452274887542));
#11888=CARTESIAN_POINT('Ctrl Pts',(0.16974114070921,0.0458437505588112,
0.0259395740526599));
#11889=CARTESIAN_POINT('Ctrl Pts',(0.166648931992492,-0.00924353559174104,
0.0222339206165656));
#11890=CARTESIAN_POINT('Ctrl Pts',(0.163556723275773,-0.0643308217422941,
0.0185282671804714));
#11891=CARTESIAN_POINT('Ctrl Pts',(0.130351962474636,-0.117782645232805,
0.0148226137443772));
#11892=CARTESIAN_POINT('Ctrl Pts',(0.0825007717953625,-0.145037847677429,
0.0111169603082829));
#11893=CARTESIAN_POINT('Ctrl Pts',(0.0346495811160894,-0.172293050122053,
0.00741130687218866));
#11894=CARTESIAN_POINT('Ctrl Pts',(-0.0278480394413196,-0.17335163152079,
0.00370565343609431));
#11895=CARTESIAN_POINT('Ctrl Pts',(-0.0769902040670456,-0.147743251885542,
5.89805981832114E-17));
#11896=CARTESIAN_POINT('Origin',(0.,0.,0.));
#11897=CARTESIAN_POINT('Ctrl Pts',(-0.166448982935848,-0.000123056367485261,
0.00714803633902118));
#11898=CARTESIAN_POINT('Ctrl Pts',(-0.166570210461424,-0.018901335955032,
0.00840082062938137));
#11899=CARTESIAN_POINT('Ctrl Pts',(-0.163628378559591,-0.03763949574471,
0.00965360491974155));
#11900=CARTESIAN_POINT('Ctrl Pts',(-0.157450514586768,-0.0552386959973693,
0.0109063892101017));
#11901=CARTESIAN_POINT('Ctrl Pts',(-0.139176799762301,-0.107295971452211,
0.014612042646196));
#11902=CARTESIAN_POINT('Ctrl Pts',(-0.0925898286465717,-0.149388063444853,
0.0183176960822903));
#11903=CARTESIAN_POINT('Ctrl Pts',(-0.0389605451714495,-0.162261019033932,
0.0220233495183846));
#11904=CARTESIAN_POINT('Ctrl Pts',(0.0146687383036719,-0.175133974623011,
0.0257290029544788));
#11905=CARTESIAN_POINT('Ctrl Pts',(0.0753403341381858,-0.158787793808527,
0.029434656390573));
#11906=CARTESIAN_POINT('Ctrl Pts',(0.115241327743874,-0.120696966553578,
0.0331403098266672));
#11907=CARTESIAN_POINT('Ctrl Pts',(0.155142321349563,-0.0826061392986276,
0.0368459632627615));
#11908=CARTESIAN_POINT('Ctrl Pts',(0.174272712726426,-0.0227706656032114,
0.0405516166988558));
#11909=CARTESIAN_POINT('Ctrl Pts',(0.163889373105412,0.0314056858317542,
0.04425727013495));
#11910=CARTESIAN_POINT('Ctrl Pts',(0.153506033484398,0.0855820372667198,
0.0479629235710443));
#11911=CARTESIAN_POINT('Ctrl Pts',(0.113608962865507,0.134099266441235,
0.0516685770071386));
#11912=CARTESIAN_POINT('Ctrl Pts',(0.0624581433490313,0.154744419673635,
0.0553742304432329));
#11913=CARTESIAN_POINT('Ctrl Pts',(0.011307323832556,0.175389572906036,
0.0590798838793272));
#11914=CARTESIAN_POINT('Ctrl Pts',(-0.0510972445815037,0.168162650196322,
0.0627855373154215));
#11915=CARTESIAN_POINT('Ctrl Pts',(-0.0961762851695443,0.136371337065745,
0.0664911907515157));
#11916=CARTESIAN_POINT('Ctrl Pts',(-0.139389570227485,0.105895819868462,
0.0700434726140175));
#11917=CARTESIAN_POINT('Ctrl Pts',(-0.166681805131909,0.052847201533458,
0.0735957544765193));
#11918=CARTESIAN_POINT('Ctrl Pts',(-0.166860410748999,-4.21553466717637E-5,
0.0771480363390211));
#11919=CARTESIAN_POINT('Origin',(0.,0.,0.2));
#11920=CARTESIAN_POINT('',(-0.166562721528158,0.000151999276579301,0.147148036339021));
#11921=CARTESIAN_POINT('',(-0.166326519955886,-5.91534338763107E-7,0.127851963660979));
#11922=CARTESIAN_POINT('',(-0.1666,2.04026156737949E-17,0.2));
#11923=CARTESIAN_POINT('Ctrl Pts',(-0.166326519955886,-5.91534338763107E-7,
0.127851963660979));
#11924=CARTESIAN_POINT('Ctrl Pts',(-0.166325716020091,0.0278480319741386,
0.12599683023769));
#11925=CARTESIAN_POINT('Ctrl Pts',(-0.159710002166229,0.0556970392585184,
0.1241416968144));
#11926=CARTESIAN_POINT('Ctrl Pts',(-0.146481565318128,0.079937430264998,
0.122286563391111));
#11927=CARTESIAN_POINT('Ctrl Pts',(-0.120057588559947,0.128357930428352,
0.118580909955017));
#11928=CARTESIAN_POINT('Ctrl Pts',(-0.0672484579299266,0.16237983929433,
0.114875256518922));
#11929=CARTESIAN_POINT('Ctrl Pts',(-0.0122358634786086,0.166424502517241,
0.111169603082828));
#11930=CARTESIAN_POINT('Ctrl Pts',(0.0427767309727098,0.170469165740151,
0.107463949646734));
#11931=CARTESIAN_POINT('Ctrl Pts',(0.0999927892453255,0.144536583319994,
0.10375829621064));
#11932=CARTESIAN_POINT('Ctrl Pts',(0.133214635576823,0.100501528314839,
0.100052642774545));
#11933=CARTESIAN_POINT('Ctrl Pts',(0.16643648190832,0.0564664733096838,
0.096346989338451));
#11934=CARTESIAN_POINT('Ctrl Pts',(0.175664116298698,-0.00567105428046926,
0.0926413359023568));
#11935=CARTESIAN_POINT('Ctrl Pts',(0.156669843600291,-0.0574593209837368,
0.0889356824662625));
#11936=CARTESIAN_POINT('Ctrl Pts',(0.137675570901885,-0.109247587687005,
0.0852300290301683));
#11937=CARTESIAN_POINT('Ctrl Pts',(0.0904593911146922,-0.150686593503387,
0.0815243755940739));
#11938=CARTESIAN_POINT('Ctrl Pts',(0.0366459467445889,-0.162800257272089,
0.0778187221579796));
#11939=CARTESIAN_POINT('Ctrl Pts',(-0.0171674976255144,-0.17491392104079,
0.0741130687218853));
#11940=CARTESIAN_POINT('Ctrl Pts',(-0.0775782065785286,-0.157702242761811,
0.0704074152857911));
#11941=CARTESIAN_POINT('Ctrl Pts',(-0.11693320189458,-0.119048983744838,
0.0667017618496969));
#11942=CARTESIAN_POINT('Ctrl Pts',(-0.148262248379121,-0.0882785634005673,
0.0637518291201243));
#11943=CARTESIAN_POINT('Ctrl Pts',(-0.166247953720068,-0.0439202717840205,
0.0608018963905518));
#11944=CARTESIAN_POINT('Ctrl Pts',(-0.166654775959782,0.000146646548331295,
0.0578519636609792));
#11945=CARTESIAN_POINT('Ctrl Pts',(-0.166860410748999,-4.21553466717637E-5,
0.0771480363390211));
#11946=CARTESIAN_POINT('Ctrl Pts',(-0.166868122137229,-0.00232568019210335,
0.0773014079126136));
#11947=CARTESIAN_POINT('Ctrl Pts',(-0.166825290345314,-0.00460890815435789,
0.077454779486206));
#11948=CARTESIAN_POINT('Ctrl Pts',(-0.16673101454388,-0.00689000963011461,
0.0776081510597985));
#11949=CARTESIAN_POINT('Ctrl Pts',(-0.164453190568154,-0.0620043396439587,
0.0813138044958928));
#11950=CARTESIAN_POINT('Ctrl Pts',(-0.13214402985468,-0.115877296120208,
0.0850194579319871));
#11951=CARTESIAN_POINT('Ctrl Pts',(-0.0845964830895265,-0.143841137535084,
0.0887251113680814));
#11952=CARTESIAN_POINT('Ctrl Pts',(-0.0370489363243729,-0.17180497894996,
0.0924307648041757));
#11953=CARTESIAN_POINT('Ctrl Pts',(0.0257369964924607,-0.173859705303464,
0.0961364182402699));
#11954=CARTESIAN_POINT('Ctrl Pts',(0.0750113070876087,-0.149064254577995,
0.0998420716763641));
#11955=CARTESIAN_POINT('Ctrl Pts',(0.124285617682757,-0.124268803852526,
0.103547725112458));
#11956=CARTESIAN_POINT('Ctrl Pts',(0.160048306056219,-0.0726231760480842,
0.107253378548553));
#11957=CARTESIAN_POINT('Ctrl Pts',(0.165924163852847,-0.01777574960003,
0.110959031984647));
#11958=CARTESIAN_POINT('Ctrl Pts',(0.171800021649474,0.0370716768480245,
0.114664685420741));
#11959=CARTESIAN_POINT('Ctrl Pts',(0.147789048869266,0.0951209019396915,
0.118370338856835));
#11960=CARTESIAN_POINT('Ctrl Pts',(0.104885566869347,0.129791543346377,
0.12207599229293));
#11961=CARTESIAN_POINT('Ctrl Pts',(0.0619820848694269,0.164462184753062,
0.125781645729024));
#11962=CARTESIAN_POINT('Ctrl Pts',(0.000186093649795584,0.175754242474766,
0.129487299165118));
#11963=CARTESIAN_POINT('Ctrl Pts',(-0.052206247152358,0.158497110915842,
0.133192952601213));
#11964=CARTESIAN_POINT('Ctrl Pts',(-0.104598587954512,0.141239979356918,
0.136898606037307));
#11965=CARTESIAN_POINT('Ctrl Pts',(-0.147587278339187,0.0954336585173664,
0.140604259473401));
#11966=CARTESIAN_POINT('Ctrl Pts',(-0.161488067840993,0.0420526424254004,
0.144309912909495));
#11967=CARTESIAN_POINT('Ctrl Pts',(-0.165036893714247,0.0284246444600193,
0.145255954052671));
#11968=CARTESIAN_POINT('Ctrl Pts',(-0.16668987457928,0.0143029550371173,
0.146201995195846));
#11969=CARTESIAN_POINT('Ctrl Pts',(-0.166562721528158,0.000151999276579301,
0.147148036339021));
#11970=CARTESIAN_POINT('Origin',(0.,0.,0.2));
#11971=CARTESIAN_POINT('',(-0.166338651274879,-4.67853121875056E-5,0.217148036339021));
#11972=CARTESIAN_POINT('',(-0.166650872726138,-0.000148155484504217,0.197851963660979));
#11973=CARTESIAN_POINT('',(-0.1666,2.04026156737949E-17,0.2));
#11974=CARTESIAN_POINT('Ctrl Pts',(-0.166650872726138,-0.000148155484504217,
0.197851963660979));
#11975=CARTESIAN_POINT('Ctrl Pts',(-0.16624400073373,0.0439863598254954,
0.194897417520922));
#11976=CARTESIAN_POINT('Ctrl Pts',(-0.148202282970397,0.0884148461429154,
0.191942871380865));
#11977=CARTESIAN_POINT('Ctrl Pts',(-0.116787784478103,0.119194926752247,
0.188988325240808));
#11978=CARTESIAN_POINT('Ctrl Pts',(-0.0773870647862129,0.157799946293768,
0.185282671804713));
#11979=CARTESIAN_POINT('Ctrl Pts',(-0.0169500249703049,0.174935068326537,
0.181577018368619));
#11980=CARTESIAN_POINT('Ctrl Pts',(0.0368495126734258,0.162754204250394,
0.177871364932525));
#11981=CARTESIAN_POINT('Ctrl Pts',(0.0906490503171566,0.150573340174251,
0.174165711496431));
#11982=CARTESIAN_POINT('Ctrl Pts',(0.13781108578871,0.109076489989194,0.170460058060336));
#11983=CARTESIAN_POINT('Ctrl Pts',(0.156740392213101,0.0572648554840297,
0.166754404624242));
#11984=CARTESIAN_POINT('Ctrl Pts',(0.175669698637491,0.00545322097886432,
0.163048751188148));
#11985=CARTESIAN_POINT('Ctrl Pts',(0.166366276014719,-0.0566731978464093,
0.159343097752054));
#11986=CARTESIAN_POINT('Ctrl Pts',(0.133090063801353,-0.100667049200161,
0.155637444315959));
#11987=CARTESIAN_POINT('Ctrl Pts',(0.0998138515879878,-0.144660900553913,
0.151931790879865));
#11988=CARTESIAN_POINT('Ctrl Pts',(0.042564849784029,-0.170522184436142,
0.148226137443771));
#11989=CARTESIAN_POINT('Ctrl Pts',(-0.0124428237561262,-0.166409123794165,
0.144520484007676));
#11990=CARTESIAN_POINT('Ctrl Pts',(-0.0674504972962818,-0.162296063152188,
0.140814830571582));
#11991=CARTESIAN_POINT('Ctrl Pts',(-0.120216842572635,-0.128208657986004,
0.137109177135488));
#11992=CARTESIAN_POINT('Ctrl Pts',(-0.146580603767641,-0.0797554096725464,
0.133403523699394));
#11993=CARTESIAN_POINT('Ctrl Pts',(-0.159746073379281,-0.0555589468257773,
0.131553003686589));
#11994=CARTESIAN_POINT('Ctrl Pts',(-0.166327321892425,-0.0277799601148087,
0.129702483673784));
#11995=CARTESIAN_POINT('Ctrl Pts',(-0.166326519955886,-5.91534338763107E-7,
0.127851963660979));
#11996=CARTESIAN_POINT('Ctrl Pts',(-0.166562721528158,0.000151999276579301,
0.147148036339021));
#11997=CARTESIAN_POINT('Ctrl Pts',(-0.166191814696579,-0.0411264924201606,
0.14990764863194));
#11998=CARTESIAN_POINT('Ctrl Pts',(-0.150673833135845,-0.0826540099902898,
0.152667260924859));
#11999=CARTESIAN_POINT('Ctrl Pts',(-0.122880807906595,-0.112903193819225,
0.155426873217778));
#12000=CARTESIAN_POINT('Ctrl Pts',(-0.0855598698514573,-0.153522302627504,
0.159132526653873));
#12001=CARTESIAN_POINT('Ctrl Pts',(-0.026105105122248,-0.173804808899682,
0.162838180089967));
#12002=CARTESIAN_POINT('Ctrl Pts',(0.0282594425548545,-0.164463453749595,
0.166543833526061));
#12003=CARTESIAN_POINT('Ctrl Pts',(0.0826239902319573,-0.155122098599507,
0.170249486962155));
#12004=CARTESIAN_POINT('Ctrl Pts',(0.131898320856954,-0.116156882027153,
0.17395514039825));
#12005=CARTESIAN_POINT('Ctrl Pts',(0.153519979653527,-0.0654097770223532,
0.177660793834344));
#12006=CARTESIAN_POINT('Ctrl Pts',(0.1751416384501,-0.0146626720175531,
0.181366447270438));
#12007=CARTESIAN_POINT('Ctrl Pts',(0.169110625418251,0.0478663214196927,
0.185072100706532));
#12008=CARTESIAN_POINT('Ctrl Pts',(0.138188506492137,0.093545498793948,
0.188777754142626));
#12009=CARTESIAN_POINT('Ctrl Pts',(0.107266387566023,0.139224676168203,
0.192483407578721));
#12010=CARTESIAN_POINT('Ctrl Pts',(0.0514531627456449,0.168054037479467,
0.196189061014815));
#12011=CARTESIAN_POINT('Ctrl Pts',(-0.00369457792842184,0.166832770092881,
0.199894714450909));
#12012=CARTESIAN_POINT('Ctrl Pts',(-0.0588423186024886,0.165611502706295,
0.203600367887004));
#12013=CARTESIAN_POINT('Ctrl Pts',(-0.113324575130244,0.134339606621858,
0.207306021323098));
#12014=CARTESIAN_POINT('Ctrl Pts',(-0.142194204679298,0.0873363147171791,
0.211011674759192));
#12015=CARTESIAN_POINT('Ctrl Pts',(-0.15812971948515,0.0613913453576635,
0.213057128619135));
#12016=CARTESIAN_POINT('Ctrl Pts',(-0.166261474396152,0.0306532700081179,
0.215102582479078));
#12017=CARTESIAN_POINT('Ctrl Pts',(-0.166338651274879,-4.67853121875056E-5,
0.217148036339021));
#12018=CARTESIAN_POINT('Origin',(0.,0.,0.2));
#12019=CARTESIAN_POINT('',(-0.166734374774229,-0.000128818837332453,0.287148036339021));
#12020=CARTESIAN_POINT('',(-0.166813199754551,8.97901853038408E-5,0.267851963660979));
#12021=CARTESIAN_POINT('',(-0.1666,2.04026156737949E-17,0.2));
#12022=CARTESIAN_POINT('Ctrl Pts',(-0.166813199754551,8.97901853038408E-5,
0.267851963660979));
#12023=CARTESIAN_POINT('Ctrl Pts',(-0.166846982879129,0.00527956240150659,
0.267503658240248));
#12024=CARTESIAN_POINT('Ctrl Pts',(-0.166625794764039,0.0104664167280576,
0.267155352819518));
#12025=CARTESIAN_POINT('Ctrl Pts',(-0.166140220809639,0.0156284006424284,
0.266807047398787));
#12026=CARTESIAN_POINT('Ctrl Pts',(-0.16097415480692,0.070547222718839,
0.263101393962693));
#12027=CARTESIAN_POINT('Ctrl Pts',(-0.125882181662303,0.122650955880377,
0.259395740526599));
#12028=CARTESIAN_POINT('Ctrl Pts',(-0.0769327614968034,0.148081614095739,
0.255690087090505));
#12029=CARTESIAN_POINT('Ctrl Pts',(-0.027983341331303,0.173512272311101,
0.25198443365441));
#12030=CARTESIAN_POINT('Ctrl Pts',(0.0348235258550809,0.172269855580289,
0.248278780218316));
#12031=CARTESIAN_POINT('Ctrl Pts',(0.0827289131521439,0.144923236625853,
0.244573126782222));
#12032=CARTESIAN_POINT('Ctrl Pts',(0.130634300449207,0.117576617671417,
0.240867473346127));
#12033=CARTESIAN_POINT('Ctrl Pts',(0.163638207856949,0.064125796493358,
0.237161819910033));
#12034=CARTESIAN_POINT('Ctrl Pts',(0.166628309560831,0.00904564092131411,
0.233456166473939));
#12035=CARTESIAN_POINT('Ctrl Pts',(0.169618411264713,-0.0460345146507298,
0.229750513037845));
#12036=CARTESIAN_POINT('Ctrl Pts',(0.142594707264736,-0.102744004616759,
0.22604485960175));
#12037=CARTESIAN_POINT('Ctrl Pts',(0.0979312150883438,-0.135115852675218,
0.222339206165656));
#12038=CARTESIAN_POINT('Ctrl Pts',(0.0532677229119514,-0.167487700733677,
0.218633552729562));
#12039=CARTESIAN_POINT('Ctrl Pts',(-0.00903555744085632,-0.175521906884566,
0.214927899293468));
#12040=CARTESIAN_POINT('Ctrl Pts',(-0.0604502752026059,-0.155539645602405,
0.211222245857373));
#12041=CARTESIAN_POINT('Ctrl Pts',(-0.111864992964356,-0.135557384320243,
0.207516592421279));
#12042=CARTESIAN_POINT('Ctrl Pts',(-0.152391148135047,-0.0875586556050303,
0.203810938985185));
#12043=CARTESIAN_POINT('Ctrl Pts',(-0.163472025936457,-0.0335218327222879,
0.20010528554909));
#12044=CARTESIAN_POINT('Ctrl Pts',(-0.165718034179448,-0.0225689865854744,
0.199354178253053));
#12045=CARTESIAN_POINT('Ctrl Pts',(-0.166754308078833,-0.0113680704511269,
0.198603070957016));
#12046=CARTESIAN_POINT('Ctrl Pts',(-0.166650872726138,-0.000148155484504217,
0.197851963660979));
#12047=CARTESIAN_POINT('Ctrl Pts',(-0.166338651274879,-4.67853121875056E-5,
0.217148036339021));
#12048=CARTESIAN_POINT('Ctrl Pts',(-0.166401292150756,-0.0249645895358502,
0.218808235915172));
#12049=CARTESIAN_POINT('Ctrl Pts',(-0.16115772813329,-0.0498573468775544,
0.220468435491324));
#12050=CARTESIAN_POINT('Ctrl Pts',(-0.150473846254983,-0.0721418444426733,
0.222128635067475));
#12051=CARTESIAN_POINT('Ctrl Pts',(-0.126626855711259,-0.121882023972926,
0.225834288503569));
#12052=CARTESIAN_POINT('Ctrl Pts',(-0.0756758720534593,-0.158627695308512,
0.229539941939664));
#12053=CARTESIAN_POINT('Ctrl Pts',(-0.0209510900103489,-0.165553231974957,
0.233245595375758));
#12054=CARTESIAN_POINT('Ctrl Pts',(0.0337736920327618,-0.172478768641402,
0.236951248811852));
#12055=CARTESIAN_POINT('Ctrl Pts',(0.0922722724611822,-0.149584170638707,
0.240656902247946));
#12056=CARTESIAN_POINT('Ctrl Pts',(0.127758456442371,-0.107352704753372,
0.244362555684041));
#12057=CARTESIAN_POINT('Ctrl Pts',(0.16324464042356,-0.0651212388680367,
0.248068209120135));
#12058=CARTESIAN_POINT('Ctrl Pts',(0.175718427957517,-0.00355290510006166,
0.251773862556229));
#12059=CARTESIAN_POINT('Ctrl Pts',(0.159468129568603,0.0491603754423182,
0.255479515992324));
#12060=CARTESIAN_POINT('Ctrl Pts',(0.14321783117969,0.101873655984698,0.259185169428418));
#12061=CARTESIAN_POINT('Ctrl Pts',(0.0982434468679055,0.145731883301483,
0.262890822864512));
#12062=CARTESIAN_POINT('Ctrl Pts',(0.045138527575508,0.160652789432442,
0.266596476300606));
#12063=CARTESIAN_POINT('Ctrl Pts',(-0.00796639171688973,0.1755736955634,
0.2703021297367));
#12064=CARTESIAN_POINT('Ctrl Pts',(-0.0692018459899008,0.161557280508531,
0.274007783172795));
#12065=CARTESIAN_POINT('Ctrl Pts',(-0.110528459862841,0.125021229174222,
0.277713436608889));
#12066=CARTESIAN_POINT('Ctrl Pts',(-0.145601002111859,0.0940142802871293,
0.2808583031856));
#12067=CARTESIAN_POINT('Ctrl Pts',(-0.166334479996432,0.0467878777510125,
0.28400316976231));
#12068=CARTESIAN_POINT('Ctrl Pts',(-0.166734374774229,-0.000128818837332453,
0.287148036339021));
#12069=CARTESIAN_POINT('Origin',(0.,0.,0.2));
#12070=CARTESIAN_POINT('',(-0.166743774672904,0.000120896768023321,0.357148036339021));
#12071=CARTESIAN_POINT('',(-0.166378928688253,9.26016813348553E-5,0.337851963660979));
#12072=CARTESIAN_POINT('',(-0.1666,2.04026156737949E-17,0.2));
#12073=CARTESIAN_POINT('',(0.126907087985239,0.107935865304851,0.4));
#12074=CARTESIAN_POINT('Ctrl Pts',(-0.166743774672904,0.000120896768023321,
0.357148036339021));
#12075=CARTESIAN_POINT('Ctrl Pts',(-0.166347196302146,-0.0471069253752206,
0.360315063917731));
#12076=CARTESIAN_POINT('Ctrl Pts',(-0.14528367999841,-0.0946317549803691,
0.363482091496441));
#12077=CARTESIAN_POINT('Ctrl Pts',(-0.109779302776043,-0.125660187653584,
0.366649119075152));
#12078=CARTESIAN_POINT('Ctrl Pts',(-0.0682365898755026,-0.161965718721597,
0.370354772511246));
#12079=CARTESIAN_POINT('Ctrl Pts',(-0.00692331585482878,-0.175686514319717,
0.37406042594734));
#12080=CARTESIAN_POINT('Ctrl Pts',(0.0460947087719345,-0.160413783553521,
0.377766079383434));
#12081=CARTESIAN_POINT('Ctrl Pts',(0.0991127333986977,-0.145141052787325,
0.381471732819529));
#12082=CARTESIAN_POINT('Ctrl Pts',(0.143835508631551,-0.100874795656813,
0.385177386255623));
#12083=CARTESIAN_POINT('Ctrl Pts',(0.159759468393512,-0.0481584829850476,
0.388883039691717));
#12084=CARTESIAN_POINT('Ctrl Pts',(0.175683428155473,0.00455782968671844,
0.392588693127811));
#12085=CARTESIAN_POINT('Ctrl Pts',(0.162808572446542,0.0657241978997386,
0.396294346563906));
#12086=CARTESIAN_POINT('Ctrl Pts',(0.126907087985239,0.10793586530485,0.4));
#12087=CARTESIAN_POINT('',(-0.127144355350143,0.10812641955069,0.4));
#12088=CARTESIAN_POINT('Origin',(0.,0.,0.4));
#12089=CARTESIAN_POINT('Ctrl Pts',(-0.127144402274347,0.108126457236473,
0.4));
#12090=CARTESIAN_POINT('Ctrl Pts',(-0.0920292268904173,0.149320274449966,
0.396364536929966));
#12091=CARTESIAN_POINT('Ctrl Pts',(-0.0349623149552143,0.171908313823477,
0.392729073859932));
#12092=CARTESIAN_POINT('Ctrl Pts',(0.0188177088499946,0.165794607065857,
0.389093610789898));
#12093=CARTESIAN_POINT('Ctrl Pts',(0.0736360706839233,0.159562862163704,
0.385387957353804));
#12094=CARTESIAN_POINT('Ctrl Pts',(0.125039398382612,0.12351037530068,0.38168230391771));
#12095=CARTESIAN_POINT('Ctrl Pts',(0.149523239782922,0.074090212834763,
0.377976650481616));
#12096=CARTESIAN_POINT('Ctrl Pts',(0.174007081183232,0.0246700503688466,
0.374270997045521));
#12097=CARTESIAN_POINT('Ctrl Pts',(0.171571436285164,-0.0381177876999622,
0.370565343609427));
#12098=CARTESIAN_POINT('Ctrl Pts',(0.143314434899701,-0.0854943902146281,
0.366859690173333));
#12099=CARTESIAN_POINT('Ctrl Pts',(0.115057433514238,-0.132870992729294,
0.363154036737239));
#12100=CARTESIAN_POINT('Ctrl Pts',(0.0609790756413814,-0.164836359689817,
0.359448383301144));
#12101=CARTESIAN_POINT('Ctrl Pts',(0.0058505342293925,-0.16676871854526,
0.35574272986505));
#12102=CARTESIAN_POINT('Ctrl Pts',(-0.0492780071825968,-0.168701077400703,
0.352037076428955));
#12103=CARTESIAN_POINT('Ctrl Pts',(-0.105456732133718,-0.140600428151066,
0.348331422992861));
#12104=CARTESIAN_POINT('Ctrl Pts',(-0.136966392307533,-0.0953260539355553,
0.344625769556767));
#12105=CARTESIAN_POINT('Ctrl Pts',(-0.156165914113924,-0.0677393922506487,
0.342367834258171));
#12106=CARTESIAN_POINT('Ctrl Pts',(-0.166206477852866,-0.0337765899116774,
0.340109898959575));
#12107=CARTESIAN_POINT('Ctrl Pts',(-0.166378928688253,9.26016813348553E-5,
0.337851963660979));
#12108=CARTESIAN_POINT('Origin',(0.,0.,0.554592528053768));
#12109=CARTESIAN_POINT('',(-0.205542557565044,0.000180865543328967,0.0354074719462324));
#12110=CARTESIAN_POINT('',(-0.205288744110104,-0.000151770750953058,0.0295925280537678));
#12111=CARTESIAN_POINT('',(-0.205475,1.04123167373875E-16,0.554592528053768));
#12112=CARTESIAN_POINT('',(0.181742788875946,0.0958620587959239,0.));
#12113=CARTESIAN_POINT('Ctrl Pts',(-0.205288744110104,-0.000151770750953056,
0.0295925280537678));
#12114=CARTESIAN_POINT('Ctrl Pts',(-0.204996003270372,0.0451941134373501,
0.0271396589080337));
#12115=CARTESIAN_POINT('Ctrl Pts',(-0.16789984592073,0.159522204476035,
0.0209811363262054));
#12116=CARTESIAN_POINT('Ctrl Pts',(0.0215757967252497,0.241850803896632,
0.0111169603082828));
#12117=CARTESIAN_POINT('Ctrl Pts',(0.149857277933222,0.156313104352978,
0.00370565343609428));
#12118=CARTESIAN_POINT('Ctrl Pts',(0.181742788875947,0.0958620587959227,
0.));
#12119=CARTESIAN_POINT('',(0.205712120425506,-0.00753776543806376,-7.73744768374671E-17));
#12120=CARTESIAN_POINT('Origin',(0.,0.,0.));
#12121=CARTESIAN_POINT('Ctrl Pts',(-0.205542557565044,0.000180865543328964,
0.0354074719462324));
#12122=CARTESIAN_POINT('Ctrl Pts',(-0.205671097444409,0.014104284209969,
0.0346517512397107));
#12123=CARTESIAN_POINT('Ctrl Pts',(-0.198029895298052,0.0961615295363027,
0.0301903770970948));
#12124=CARTESIAN_POINT('Ctrl Pts',(-0.0876598130547602,0.226510042114602,
0.0220233495183845));
#12125=CARTESIAN_POINT('Ctrl Pts',(0.1412439463355,0.196648073709114,0.0109765795761622));
#12126=CARTESIAN_POINT('Ctrl Pts',(0.20807884879869,0.0591805639213882,
0.00363546307003382));
#12127=CARTESIAN_POINT('Ctrl Pts',(0.205712194497466,-0.00753777023904147,
-9.75646429965393E-17));
#12128=CARTESIAN_POINT('Origin',(0.,0.,0.554592528053768));
#12129=CARTESIAN_POINT('',(-0.205137705209698,-7.29564938461991E-7,0.105407471946233));
#12130=CARTESIAN_POINT('',(-0.205796175862248,-5.19920159535992E-5,0.0995925280537679));
#12131=CARTESIAN_POINT('',(-0.205475,1.04123167373875E-16,0.554592528053768));
#12132=CARTESIAN_POINT('Ctrl Pts',(-0.205796175862248,-5.19920159536016E-5,
0.0995925280537679));
#12133=CARTESIAN_POINT('Ctrl Pts',(-0.205575893814401,0.065178743908085,
0.0960402461912661));
#12134=CARTESIAN_POINT('Ctrl Pts',(-0.136801184004399,0.198857914726747,
0.0887823108926702));
#12135=CARTESIAN_POINT('Ctrl Pts',(0.0909120711847139,0.225228838155139,
0.0778187221579794));
#12136=CARTESIAN_POINT('Ctrl Pts',(0.238532429865686,0.0457136341101189,
0.0667017618496969));
#12137=CARTESIAN_POINT('Ctrl Pts',(0.167749407629896,-0.175679414345444,
0.0555848015414138));
#12138=CARTESIAN_POINT('Ctrl Pts',(-0.056737317834033,-0.236160773940692,
0.0444678412331312));
#12139=CARTESIAN_POINT('Ctrl Pts',(-0.19107773121668,-0.114782008526112,
0.0358037500705825));
#12140=CARTESIAN_POINT('Ctrl Pts',(-0.205438259271075,-0.0233118367668669,
0.030845312344128));
#12141=CARTESIAN_POINT('Ctrl Pts',(-0.205288744110104,-0.000151770750953056,
0.0295925280537678));
#12142=CARTESIAN_POINT('Ctrl Pts',(-0.205137705209698,-7.29564938455052E-7,
0.105407471946233));
#12143=CARTESIAN_POINT('Ctrl Pts',(-0.205136713680842,0.0343461846931921,
0.103552338522943));
#12144=CARTESIAN_POINT('Ctrl Pts',(-0.180678665067047,0.137302931168816,
0.0979915516635594));
#12145=CARTESIAN_POINT('Ctrl Pts',(-0.0178086481209368,0.24223078753445,
0.0887251113680815));
#12146=CARTESIAN_POINT('Ctrl Pts',(0.193892484656356,0.146279454291081,
0.0776081510597986));
#12147=CARTESIAN_POINT('Ctrl Pts',(0.228035008840565,-0.083631262664263,
0.0664911907515159));
#12148=CARTESIAN_POINT('Ctrl Pts',(0.0533337265757384,-0.236956827852518,
0.0553742304432329));
#12149=CARTESIAN_POINT('Ctrl Pts',(-0.154992928561183,-0.177602262622348,
0.0450129908414718));
#12150=CARTESIAN_POINT('Ctrl Pts',(-0.205040806066213,-0.0541687745787603,
0.038357404675805));
#12151=CARTESIAN_POINT('Ctrl Pts',(-0.205542557565044,0.000180865543328964,
0.0354074719462324));
#12152=CARTESIAN_POINT('Origin',(0.,0.,0.554592528053768));
#12153=CARTESIAN_POINT('',(-0.205537743537834,-0.000182726579705819,0.175407471946233));
#12154=CARTESIAN_POINT('',(-0.205429022845128,0.000187467295045848,0.169592528053768));
#12155=CARTESIAN_POINT('',(-0.205475,1.04123167373875E-16,0.554592528053768));
#12156=CARTESIAN_POINT('Ctrl Pts',(-0.205429022845128,0.000187467295045865,
0.169592528053768));
#12157=CARTESIAN_POINT('Ctrl Pts',(-0.205585846213551,0.0176404542992278,
0.168646486910593));
#12158=CARTESIAN_POINT('Ctrl Pts',(-0.195561570894733,0.103279499333914,
0.163994792331323));
#12159=CARTESIAN_POINT('Ctrl Pts',(-0.0759861566816445,0.230692308120466,
0.155637444315959));
#12160=CARTESIAN_POINT('Ctrl Pts',(0.152660865452576,0.188911355652872,
0.144520484007676));
#12161=CARTESIAN_POINT('Ctrl Pts',(0.241502185356776,-0.0258725193599183,
0.133403523699394));
#12162=CARTESIAN_POINT('Ctrl Pts',(0.109179165064989,-0.216962892225182,
0.122286563391111));
#12163=CARTESIAN_POINT('Ctrl Pts',(-0.123130670689012,-0.209360343050761,
0.111169603082828));
#12164=CARTESIAN_POINT('Ctrl Pts',(-0.204476509229018,-0.0737226253751628,
0.103604924637047));
#12165=CARTESIAN_POINT('Ctrl Pts',(-0.205805686651544,-0.00286836216970447,
0.0997458996273603));
#12166=CARTESIAN_POINT('Ctrl Pts',(-0.205796175862248,-5.19920159536016E-5,
0.0995925280537679));
#12167=CARTESIAN_POINT('Ctrl Pts',(-0.205537743537834,-0.00018272657970583,
0.175407471946233));
#12168=CARTESIAN_POINT('Ctrl Pts',(-0.20503593067685,0.0542502838243898,
0.172452925806175));
#12169=CARTESIAN_POINT('Ctrl Pts',(-0.154875836490767,0.177771618514381,
0.165792726230024));
#12170=CARTESIAN_POINT('Ctrl Pts',(0.0536344200204105,0.236888489580304,
0.155426873217778));
#12171=CARTESIAN_POINT('Ctrl Pts',(0.228135366692393,0.0833488984919273,
0.144309912909495));
#12172=CARTESIAN_POINT('Ctrl Pts',(0.193712423773769,-0.146520715699965,
0.133192952601213));
#12173=CARTESIAN_POINT('Ctrl Pts',(-0.0181106010581924,-0.24220824221319,
0.12207599229293));
#12174=CARTESIAN_POINT('Ctrl Pts',(-0.18076764144762,-0.137130727182572,
0.112814165407936));
#12175=CARTESIAN_POINT('Ctrl Pts',(-0.205138694272785,-0.0342622287190314,
0.107257991959037));
#12176=CARTESIAN_POINT('Ctrl Pts',(-0.205137705209698,-7.29564938455052E-7,
0.105407471946233));
#12177=CARTESIAN_POINT('Origin',(0.,0.,0.554592528053768));
#12178=CARTESIAN_POINT('',(-0.205737948496796,0.000110742126799651,0.245407471946232));
#12179=CARTESIAN_POINT('',(-0.205152667291151,-5.77023530759702E-5,0.239592528053768));
#12180=CARTESIAN_POINT('',(-0.205475,1.04123167373875E-16,0.554592528053768));
#12181=CARTESIAN_POINT('Ctrl Pts',(-0.205152667291151,-5.77023530759641E-5,
0.239592528053768));
#12182=CARTESIAN_POINT('Ctrl Pts',(-0.205057481701977,0.0378060063320381,
0.237547074193825));
#12183=CARTESIAN_POINT('Ctrl Pts',(-0.17685871883546,0.144397474870061,
0.231795966897788));
#12184=CARTESIAN_POINT('Ctrl Pts',(-0.00537745351023951,0.242824828130405,
0.222339206165656));
#12185=CARTESIAN_POINT('Ctrl Pts',(0.201133153391932,0.136155326051799,
0.211222245857373));
#12186=CARTESIAN_POINT('Ctrl Pts',(0.223448082612567,-0.0952038262864637,
0.20010528554909));
#12187=CARTESIAN_POINT('Ctrl Pts',(0.0411315804786337,-0.23937629702844,
0.188988325240808));
#12188=CARTESIAN_POINT('Ctrl Pts',(-0.160132400758511,-0.170716737438922,
0.1788174060757));
#12189=CARTESIAN_POINT('Ctrl Pts',(-0.204971567375627,-0.0507230854143627,
0.172352140346687));
#12190=CARTESIAN_POINT('Ctrl Pts',(-0.205429022845128,0.000187467295045865,
0.169592528053768));
#12191=CARTESIAN_POINT('Ctrl Pts',(-0.205737948496796,0.00011074212679966,
0.245407471946232));
#12192=CARTESIAN_POINT('Ctrl Pts',(-0.205779614688409,0.00651151311194001,
0.245059166525502));
#12193=CARTESIAN_POINT('Ctrl Pts',(-0.202604460038461,0.0809687895657837,
0.241005207668677));
#12194=CARTESIAN_POINT('Ctrl Pts',(-0.111975498770539,0.215532531397883,
0.233245595375758));
#12195=CARTESIAN_POINT('Ctrl Pts',(0.120411794779082,0.210935552206459,
0.222128635067475));
#12196=CARTESIAN_POINT('Ctrl Pts',(0.242527242701154,0.0131659096813392,
0.211011674759192));
#12197=CARTESIAN_POINT('Ctrl Pts',(0.142538726865704,-0.196660905158453,
0.199894714450909));
#12198=CARTESIAN_POINT('Ctrl Pts',(-0.087985280286033,-0.226387709039377,
0.188777754142627));
#12199=CARTESIAN_POINT('Ctrl Pts',(-0.198081706594962,-0.0959907227805277,
0.180615339974401));
#12200=CARTESIAN_POINT('Ctrl Pts',(-0.205665314840926,-0.0140207339492534,
0.17615857924227));
#12201=CARTESIAN_POINT('Ctrl Pts',(-0.205537743537834,-0.00018272657970583,
0.175407471946233));
#12202=CARTESIAN_POINT('Origin',(0.,0.,0.554592528053768));
#12203=CARTESIAN_POINT('',(-0.205202343170581,0.000114209666698867,0.315407471946233));
#12204=CARTESIAN_POINT('',(-0.205640730232501,-0.000158877854750073,0.309592528053768));
#12205=CARTESIAN_POINT('',(-0.205475,1.04123167373875E-16,0.554592528053768));
#12206=CARTESIAN_POINT('Ctrl Pts',(-0.205640730232501,-0.000158877854750081,
0.309592528053768));
#12207=CARTESIAN_POINT('Ctrl Pts',(-0.205147522672671,0.0577055172922507,
0.306447661477057));
#12208=CARTESIAN_POINT('Ctrl Pts',(-0.149444666487041,0.184584641155565,
0.299597141464252));
#12209=CARTESIAN_POINT('Ctrl Pts',(0.0656990433896697,0.233829699755635,
0.289040968015353));
#12210=CARTESIAN_POINT('Ctrl Pts',(0.232105615114709,0.0715529424102004,
0.27792400770707));
#12211=CARTESIAN_POINT('Ctrl Pts',(0.185952226875698,-0.156251740320434,
0.266807047398788));
#12212=CARTESIAN_POINT('Ctrl Pts',(-0.030494276369136,-0.240962440043193,
0.255690087090504));
#12213=CARTESIAN_POINT('Ctrl Pts',(-0.18432786741861,-0.130018191841,0.246618580642165));
#12214=CARTESIAN_POINT('Ctrl Pts',(-0.205229924998058,-0.0307899101733451,
0.241252727629919));
#12215=CARTESIAN_POINT('Ctrl Pts',(-0.205152667291151,-5.77023530759641E-5,
0.239592528053768));
#12216=CARTESIAN_POINT('Ctrl Pts',(-0.205202343170581,0.000114209666698874,
0.315407471946233));
#12217=CARTESIAN_POINT('Ctrl Pts',(-0.205338714105211,0.0268973406518496,
0.313959753808734));
#12218=CARTESIAN_POINT('Ctrl Pts',(-0.188013873562118,0.122066992862534,
0.308806382235141));
#12219=CARTESIAN_POINT('Ctrl Pts',(-0.0442230349178335,0.238822732453524,
0.299947357225455));
#12220=CARTESIAN_POINT('Ctrl Pts',(0.176712068309585,0.166630571298318,
0.288830396917172));
#12221=CARTESIAN_POINT('Ctrl Pts',(0.235817802334529,-0.0581630255277868,
0.277713436608889));
#12222=CARTESIAN_POINT('Ctrl Pts',(0.078963123396891,-0.229690015875461,
0.266596476300606));
#12223=CARTESIAN_POINT('Ctrl Pts',(-0.143024641581339,-0.192086316597046,
0.255827821413055));
#12224=CARTESIAN_POINT('Ctrl Pts',(-0.205336324240059,-0.0615868786529226,
0.248764819961596));
#12225=CARTESIAN_POINT('Ctrl Pts',(-0.205737948496796,0.00011074212679966,
0.245407471946232));
#12226=CARTESIAN_POINT('Origin',(0.,0.,0.554592528053768));
#12227=CARTESIAN_POINT('',(-0.205269929560708,-0.000254221530507082,0.385407471946233));
#12228=CARTESIAN_POINT('',(-0.205652323534904,0.00014910722334396,0.379592528053768));
#12229=CARTESIAN_POINT('',(-0.205475,1.04123167373875E-16,0.554592528053768));
#12230=CARTESIAN_POINT('',(-0.053017021718863,-0.198517432567172,0.4));
#12231=CARTESIAN_POINT('Ctrl Pts',(-0.0530170217188623,-0.198517432567172,
0.4));
#12232=CARTESIAN_POINT('Ctrl Pts',(-0.11904762702766,-0.180882981070921,
0.396294346563906));
#12233=CARTESIAN_POINT('Ctrl Pts',(-0.192514897068364,-0.111293028538514,
0.391430170545983));
#12234=CARTESIAN_POINT('Ctrl Pts',(-0.205432812329624,-0.0216624454594562,
0.386565994528061));
#12235=CARTESIAN_POINT('Ctrl Pts',(-0.205269929560708,-0.000254221530507089,
0.385407471946233));
#12236=CARTESIAN_POINT('',(0.0531240965569158,-0.198877135945741,0.4));
#12237=CARTESIAN_POINT('Origin',(0.,0.,0.4));
#12238=CARTESIAN_POINT('Ctrl Pts',(0.0531241180331692,-0.198877208092298,
0.4));
#12239=CARTESIAN_POINT('Ctrl Pts',(-0.0113947906349914,-0.216030727448873,
0.396364536929966));
#12240=CARTESIAN_POINT('Ctrl Pts',(-0.149363620668702,-0.183997545270092,
0.389562046281222));
#12241=CARTESIAN_POINT('Ctrl Pts',(-0.205163206243598,-0.0580990125538643,
0.382759555632478));
#12242=CARTESIAN_POINT('Ctrl Pts',(-0.205652323534904,0.000149107223343921,
0.379592528053768));
#12243=CARTESIAN_POINT('Origin',(0.,0.,0.554592528053768));
#12244=CARTESIAN_POINT('Ctrl Pts',(-0.205652323534904,0.000149107223343921,
0.379592528053768));
#12245=CARTESIAN_POINT('Ctrl Pts',(-0.20573550917628,0.010055539256624,
0.379053902196384));
#12246=CARTESIAN_POINT('Ctrl Pts',(-0.200581379579465,0.0880330322633288,
0.374809622902905));
#12247=CARTESIAN_POINT('Ctrl Pts',(-0.100785874709386,0.221009791285371,
0.366859690173332));
#12248=CARTESIAN_POINT('Ctrl Pts',(0.131058487025979,0.204477699076557,
0.35574272986505));
#12249=CARTESIAN_POINT('Ctrl Pts',(0.242883715861565,0.000731295485493303,
0.344625769556767));
#12250=CARTESIAN_POINT('Ctrl Pts',(0.13227703569284,-0.20370800021477,0.333508809248484));
#12251=CARTESIAN_POINT('Ctrl Pts',(-0.0994668003959092,-0.221581469162487,
0.322391848940201));
#12252=CARTESIAN_POINT('Ctrl Pts',(-0.200331019397092,-0.0888856881277869,
0.314419755208629));
#12253=CARTESIAN_POINT('Ctrl Pts',(-0.205728678103024,-0.0104771510256757,
0.310153314913151));
#12254=CARTESIAN_POINT('Ctrl Pts',(-0.205640730232501,-0.000158877854750081,
0.309592528053768));
#12255=CARTESIAN_POINT('Ctrl Pts',(-0.205269929560708,-0.000254221530507089,
0.385407471946233));
#12256=CARTESIAN_POINT('Ctrl Pts',(-0.204911815068299,0.046813956992531,
0.382860341091967));
#12257=CARTESIAN_POINT('Ctrl Pts',(-0.165590599079174,0.163076528415273,
0.376607556801606));
#12258=CARTESIAN_POINT('Ctrl Pts',(0.0274206054315193,0.241260887402562,
0.366649119075152));
#12259=CARTESIAN_POINT('Ctrl Pts',(0.217614460633585,0.107865604001965,
0.355532158766869));
#12260=CARTESIAN_POINT('Ctrl Pts',(0.208602501412145,-0.124451281241526,
0.344415198458586));
#12261=CARTESIAN_POINT('Ctrl Pts',(0.00851095428263868,-0.242724098340208,
0.333298238150303));
#12262=CARTESIAN_POINT('Ctrl Pts',(-0.172282834993387,-0.152290880723065,
0.323628995979519));
#12263=CARTESIAN_POINT('Ctrl Pts',(-0.204989652081738,-0.0416581321254629,
0.317665407244829));
#12264=CARTESIAN_POINT('Ctrl Pts',(-0.205202343170581,0.000114209666698874,
0.315407471946233));
#12265=CARTESIAN_POINT('Ctrl Pts',(0.126907087985239,0.10793586530485,0.4));
#12266=CARTESIAN_POINT('Ctrl Pts',(0.162808572446542,0.0657241978997387,
0.396294346563906));
#12267=CARTESIAN_POINT('Ctrl Pts',(0.188558283864404,-0.0566085385263014,
0.388883039691717));
#12268=CARTESIAN_POINT('Ctrl Pts',(0.0543899581658451,-0.189407309917837,
0.377766079383434));
#12269=CARTESIAN_POINT('Ctrl Pts',(-0.129549863896177,-0.148244923123477,
0.366649119075152));
#12270=CARTESIAN_POINT('Ctrl Pts',(-0.194866319237398,0.0284258764902441,
0.355532158766869));
#12271=CARTESIAN_POINT('Ctrl Pts',(-0.0817176139510098,0.17919567454991,
0.344415198458586));
#12272=CARTESIAN_POINT('Ctrl Pts',(0.106262776194322,0.165791384188609,
0.333298238150303));
#12273=CARTESIAN_POINT('Ctrl Pts',(0.196931145212491,0.000592937476010039,
0.32218127784202));
#12274=CARTESIAN_POINT('Ctrl Pts',(0.107250780612859,-0.165167309092496,
0.311064317533737));
#12275=CARTESIAN_POINT('Ctrl Pts',(-0.0806481029125611,-0.179659193393213,
0.299947357225455));
#12276=CARTESIAN_POINT('Ctrl Pts',(-0.194690620681517,-0.0296261973875841,
0.288830396917171));
#12277=CARTESIAN_POINT('Ctrl Pts',(-0.130437300262912,0.147540865453661,
0.27771343660889));
#12278=CARTESIAN_POINT('Ctrl Pts',(0.0532690625561212,0.189590110618269,
0.266596476300606));
#12279=CARTESIAN_POINT('Ctrl Pts',(0.188192215491474,0.0580154286679129,
0.255479515992324));
#12280=CARTESIAN_POINT('Ctrl Pts',(0.150770852889604,-0.126689572636011,
0.24436255568404));
#12281=CARTESIAN_POINT('Ctrl Pts',(-0.0247248883956591,-0.195373366644097,
0.233245595375758));
#12282=CARTESIAN_POINT('Ctrl Pts',(-0.17757783936906,-0.0851363526373409,
0.222128635067475));
#12283=CARTESIAN_POINT('Ctrl Pts',(-0.167806831657998,0.103067710537421,
0.211011674759192));
#12284=CARTESIAN_POINT('Ctrl Pts',(-0.00436006207473383,0.196883398790731,
0.19989471445091));
#12285=CARTESIAN_POINT('Ctrl Pts',(0.163079612386402,0.110395314856939,
0.188777754142626));
#12286=CARTESIAN_POINT('Ctrl Pts',(0.18117265148195,-0.0771916654547992,
0.177660793834344));
#12287=CARTESIAN_POINT('Ctrl Pts',(0.0333496596069613,-0.194087315171861,
0.166543833526061));
#12288=CARTESIAN_POINT('Ctrl Pts',(-0.145014634580667,-0.133239796355326,
0.155426873217778));
#12289=CARTESIAN_POINT('Ctrl Pts',(-0.190575968723863,0.0496273376778148,
0.144309912909495));
#12290=CARTESIAN_POINT('Ctrl Pts',(-0.0616098975698358,0.18704630019647,
0.133192952601213));
#12291=CARTESIAN_POINT('Ctrl Pts',(0.123778076089058,0.153170127031359,
0.12207599229293));
#12292=CARTESIAN_POINT('Ctrl Pts',(0.195810994429682,-0.0209775482436421,
0.110959031984647));
#12293=CARTESIAN_POINT('Ctrl Pts',(0.0885229293092943,-0.175914431656968,
0.0998420716763641));
#12294=CARTESIAN_POINT('Ctrl Pts',(-0.099834869141207,-0.169750252596456,
0.0887251113680815));
#12295=CARTESIAN_POINT('Ctrl Pts',(-0.196762351281628,-0.00813138316770982,
0.0776081510597984));
#12296=CARTESIAN_POINT('Ctrl Pts',(-0.113501812995563,0.160935727486608,
0.0664911907515158));
#12297=CARTESIAN_POINT('Ctrl Pts',(0.0737118922466157,0.18261649561575,
0.0553742304432329));
#12298=CARTESIAN_POINT('Ctrl Pts',(0.193403104103289,0.0370648080922049,
0.0442572701349501));
#12299=CARTESIAN_POINT('Ctrl Pts',(0.136011929972701,-0.142441612994043,
0.0331403098266672));
#12300=CARTESIAN_POINT('Ctrl Pts',(-0.0460028575308428,-0.191480155437495,
0.0220233495183845));
#12301=CARTESIAN_POINT('Ctrl Pts',(-0.185763770878031,-0.0652038794595693,
0.0109063892101018));
#12302=CARTESIAN_POINT('Ctrl Pts',(-0.155645146477646,0.120863497291556,
-0.000210571098181166));
#12303=CARTESIAN_POINT('Ctrl Pts',(0.0174937473387352,0.19609365581788,
-0.0113275314064639));
#12304=CARTESIAN_POINT('Ctrl Pts',(0.121504915457719,0.126739326853418,
-0.0187388382786524));
#12305=CARTESIAN_POINT('Ctrl Pts',(0.147357822736259,0.0777253631604853,
-0.0224444917147467));
#12306=CARTESIAN_POINT('Ctrl Pts',(0.136778062465884,0.116331236980973,
0.407481497238249));
#12307=CARTESIAN_POINT('Ctrl Pts',(0.175472004327013,0.0708362991269342,
0.403775843802155));
#12308=CARTESIAN_POINT('Ctrl Pts',(0.203224556944093,-0.0610116136267615,
0.396364536929966));
#12309=CARTESIAN_POINT('Ctrl Pts',(0.0586204696178205,-0.204139621188457,
0.385247576621684));
#12310=CARTESIAN_POINT('Ctrl Pts',(-0.139626396427117,-0.159775578158341,
0.3741306163134));
#12311=CARTESIAN_POINT('Ctrl Pts',(-0.210023238325741,0.0306368727858788,
0.363013656005118));
#12312=CARTESIAN_POINT('Ctrl Pts',(-0.0880737008704687,0.19313371346173,
0.351896695696835));
#12313=CARTESIAN_POINT('Ctrl Pts',(0.114528013138208,0.178686822484592,
0.340779735388552));
#12314=CARTESIAN_POINT('Ctrl Pts',(0.212248668762182,0.000639056812504505,
0.32966277508027));
#12315=CARTESIAN_POINT('Ctrl Pts',(0.115592865639519,-0.178014206133254,
0.318545814771986));
#12316=CARTESIAN_POINT('Ctrl Pts',(-0.086921002073677,-0.193633285316304,
0.307428854463704));
#12317=CARTESIAN_POINT('Ctrl Pts',(-0.209833873740729,-0.031930555977905,
0.296311894155421));
#12318=CARTESIAN_POINT('Ctrl Pts',(-0.14058285858168,0.159016758099742,
0.285194933847138));
#12319=CARTESIAN_POINT('Ctrl Pts',(0.0574123895006371,0.204336640330724,
0.274077973538855));
#12320=CARTESIAN_POINT('Ctrl Pts',(0.202830015365886,0.0625279332486754,
0.262961013230573));
#12321=CARTESIAN_POINT('Ctrl Pts',(0.162497977551635,-0.136543628530819,
0.251844052922289));
#12322=CARTESIAN_POINT('Ctrl Pts',(-0.0266480177201514,-0.210569724443796,
0.240727092614007));
#12323=CARTESIAN_POINT('Ctrl Pts',(-0.19139004126076,-0.0917583528549811,
0.229610132305724));
#12324=CARTESIAN_POINT('Ctrl Pts',(-0.180859033700225,0.111084431720179,
0.218493171997441));
#12325=CARTESIAN_POINT('Ctrl Pts',(-0.00469919255323577,0.212197208570623,
0.207376211689158));
#12326=CARTESIAN_POINT('Ctrl Pts',(0.175764126054912,0.118981985255226,
0.196259251380876));
#12327=CARTESIAN_POINT('Ctrl Pts',(0.195264461858822,-0.083195719065354,
0.185142291072593));
#12328=CARTESIAN_POINT('Ctrl Pts',(0.0359436332308521,-0.209183642457387,
0.17402533076431));
#12329=CARTESIAN_POINT('Ctrl Pts',(-0.156294034179153,-0.143603335937786,
0.162908370456027));
#12330=CARTESIAN_POINT('Ctrl Pts',(-0.205399179576485,0.0534874072100777,
0.151791410147744));
#12331=CARTESIAN_POINT('Ctrl Pts',(-0.0664019839404387,0.201594969504469,
0.140674449839462));
#12332=CARTESIAN_POINT('Ctrl Pts',(0.133405672543564,0.165083869905196,
0.129557489531179));
#12333=CARTESIAN_POINT('Ctrl Pts',(0.21104139140538,-0.0226092052824009,
0.118440529222896));
#12334=CARTESIAN_POINT('Ctrl Pts',(0.0954083412278594,-0.189597251846372,
0.107323568914613));
#12335=CARTESIAN_POINT('Ctrl Pts',(-0.107600136323809,-0.182953616081225,
0.0962066086063303));
#12336=CARTESIAN_POINT('Ctrl Pts',(-0.212066745851603,-0.00876385119621063,
0.0850896482980474));
#12337=CARTESIAN_POINT('Ctrl Pts',(-0.12233011027488,0.173453487402658,
0.0739726879897647));
#12338=CARTESIAN_POINT('Ctrl Pts',(0.0794452852259816,0.196820609795546,
0.0628557276814818));
#12339=CARTESIAN_POINT('Ctrl Pts',(0.208446212690755,0.0399477500981762,
0.051738767373199));
#12340=CARTESIAN_POINT('Ctrl Pts',(0.146591089191766,-0.153520880111177,
0.0406218070649162));
#12341=CARTESIAN_POINT('Ctrl Pts',(-0.0495810109652396,-0.20637369493856,
0.0295048467566334));
#12342=CARTESIAN_POINT('Ctrl Pts',(-0.200212683628898,-0.0702755097396628,
0.0183878864483507));
#12343=CARTESIAN_POINT('Ctrl Pts',(-0.167751399117339,0.130264394564884,
0.00727092614006771));
#12344=CARTESIAN_POINT('Ctrl Pts',(0.0188544304675734,0.211346038510798,
-0.00384603416821501));
#12345=CARTESIAN_POINT('Ctrl Pts',(0.130955702949553,0.136597252686605,
-0.0112573410404035));
#12346=CARTESIAN_POINT('Ctrl Pts',(0.158819478116155,0.0837709283722978,
-0.0149629944764978));
#12347=CARTESIAN_POINT('Ctrl Pts',(0.146649036946528,0.124726608657095,
0.414962994476498));
#12348=CARTESIAN_POINT('Ctrl Pts',(0.188135436207484,0.0759484003541298,
0.411257341040404));
#12349=CARTESIAN_POINT('Ctrl Pts',(0.217890830023782,-0.0654146887272218,
0.403846034168215));
#12350=CARTESIAN_POINT('Ctrl Pts',(0.0628509810697956,-0.218871932459077,
0.392729073859932));
#12351=CARTESIAN_POINT('Ctrl Pts',(-0.149702928958057,-0.171306233193206,
0.38161211355165));
#12352=CARTESIAN_POINT('Ctrl Pts',(-0.225180157414084,0.0328478690815136,
0.370495153243366));
#12353=CARTESIAN_POINT('Ctrl Pts',(-0.0944297877899273,0.207071752373551,
0.359378192935084));
#12354=CARTESIAN_POINT('Ctrl Pts',(0.122793250082094,0.191582260780575,
0.348261232626801));
#12355=CARTESIAN_POINT('Ctrl Pts',(0.227566192311873,0.000685176148998803,
0.337144272318518));
#12356=CARTESIAN_POINT('Ctrl Pts',(0.12393495066618,-0.190861103174011,
0.326027312010235));
#12357=CARTESIAN_POINT('Ctrl Pts',(-0.0931939012347931,-0.207607377239396,
0.314910351701953));
#12358=CARTESIAN_POINT('Ctrl Pts',(-0.224977126799941,-0.0342349145682256,
0.303793391393669));
#12359=CARTESIAN_POINT('Ctrl Pts',(-0.150728416900449,0.170492650745823,
0.292676431085387));
#12360=CARTESIAN_POINT('Ctrl Pts',(0.0615557164451535,0.21908317004318,
0.281559470777104));
#12361=CARTESIAN_POINT('Ctrl Pts',(0.217467815240298,0.067040437829438,
0.270442510468822));
#12362=CARTESIAN_POINT('Ctrl Pts',(0.174225102213667,-0.146397684425626,
0.259325550160538));
#12363=CARTESIAN_POINT('Ctrl Pts',(-0.0285711470446437,-0.225766082243494,
0.248208589852256));
#12364=CARTESIAN_POINT('Ctrl Pts',(-0.205202243152462,-0.0983803530726217,
0.237091629543973));
#12365=CARTESIAN_POINT('Ctrl Pts',(-0.193911235742451,0.119101152902937,
0.22597466923569));
#12366=CARTESIAN_POINT('Ctrl Pts',(-0.00503832303173776,0.227511018350514,
0.214857708927407));
#12367=CARTESIAN_POINT('Ctrl Pts',(0.188448639723422,0.127568655653512,
0.203740748619124));
#12368=CARTESIAN_POINT('Ctrl Pts',(0.209356272235695,-0.0891997726759089,
0.192623788310842));
#12369=CARTESIAN_POINT('Ctrl Pts',(0.038537606854743,-0.224279969742913,
0.181506828002559));
#12370=CARTESIAN_POINT('Ctrl Pts',(-0.16757343377764,-0.153966875520245,
0.170389867694276));
#12371=CARTESIAN_POINT('Ctrl Pts',(-0.220222390429106,0.0573474767423407,
0.159272907385993));
#12372=CARTESIAN_POINT('Ctrl Pts',(-0.0711940703110417,0.216143638812467,
0.14815594707771));
#12373=CARTESIAN_POINT('Ctrl Pts',(0.14303326899807,0.176997612779034,0.137038986769428));
#12374=CARTESIAN_POINT('Ctrl Pts',(0.226271788381078,-0.0242408623211596,
0.125922026461145));
#12375=CARTESIAN_POINT('Ctrl Pts',(0.102293753146424,-0.203280072035777,
0.114805066152862));
#12376=CARTESIAN_POINT('Ctrl Pts',(-0.115365403506411,-0.196156979565993,
0.103688105844579));
#12377=CARTESIAN_POINT('Ctrl Pts',(-0.227371140421577,-0.00939631922471147,
0.0925711455362963));
#12378=CARTESIAN_POINT('Ctrl Pts',(-0.131158407554197,0.185971247318709,
0.0814541852280135));
#12379=CARTESIAN_POINT('Ctrl Pts',(0.0851786782053478,0.211024723975343,
0.0703372249197307));
#12380=CARTESIAN_POINT('Ctrl Pts',(0.22348932127822,0.0428306921041475,
0.0592202646114479));
#12381=CARTESIAN_POINT('Ctrl Pts',(0.157170248410831,-0.16460014722831,
0.048103304303165));
#12382=CARTESIAN_POINT('Ctrl Pts',(-0.0531591643996364,-0.221267234439626,
0.0369863439948823));
#12383=CARTESIAN_POINT('Ctrl Pts',(-0.214661596379765,-0.0753471400197565,
0.0258693836865995));
#12384=CARTESIAN_POINT('Ctrl Pts',(-0.179857651757032,0.139665291838212,
0.0147524233783167));
#12385=CARTESIAN_POINT('Ctrl Pts',(0.0202151135964117,0.226598421203715,
0.00363546307003391));
#12386=CARTESIAN_POINT('Ctrl Pts',(0.140406490441387,0.146455178519791,
-0.00377584380215461));
#12387=CARTESIAN_POINT('Ctrl Pts',(0.170281133496051,0.0898164935841102,
-0.00748149723824889));
#12388=CARTESIAN_POINT('Ctrl Pts',(0.156520011427173,0.133121980333218,
0.422444491714747));
#12389=CARTESIAN_POINT('Ctrl Pts',(0.200798868087955,0.0810605015813253,
0.418738838278652));
#12390=CARTESIAN_POINT('Ctrl Pts',(0.232557103103471,-0.0698177638276817,
0.411327531406463));
#12391=CARTESIAN_POINT('Ctrl Pts',(0.0670814925217709,-0.233604243729697,
0.400210571098181));
#12392=CARTESIAN_POINT('Ctrl Pts',(-0.159779461488997,-0.18283688822807,
0.389093610789898));
#12393=CARTESIAN_POINT('Ctrl Pts',(-0.240337076502428,0.0350588653771482,
0.377976650481616));
#12394=CARTESIAN_POINT('Ctrl Pts',(-0.100785874709386,0.221009791285371,
0.366859690173332));
#12395=CARTESIAN_POINT('Ctrl Pts',(0.131058487025979,0.204477699076557,
0.35574272986505));
#12396=CARTESIAN_POINT('Ctrl Pts',(0.242883715861565,0.000731295485493303,
0.344625769556767));
#12397=CARTESIAN_POINT('Ctrl Pts',(0.13227703569284,-0.20370800021477,0.333508809248484));
#12398=CARTESIAN_POINT('Ctrl Pts',(-0.0994668003959092,-0.221581469162487,
0.322391848940201));
#12399=CARTESIAN_POINT('Ctrl Pts',(-0.240120379859152,-0.0365392731585464,
0.311274888631918));
#12400=CARTESIAN_POINT('Ctrl Pts',(-0.160873975219218,0.181968543391903,
0.300157928323636));
#12401=CARTESIAN_POINT('Ctrl Pts',(0.0656990433896697,0.233829699755635,
0.289040968015353));
#12402=CARTESIAN_POINT('Ctrl Pts',(0.232105615114709,0.0715529424102004,
0.27792400770707));
#12403=CARTESIAN_POINT('Ctrl Pts',(0.185952226875698,-0.156251740320434,
0.266807047398788));
#12404=CARTESIAN_POINT('Ctrl Pts',(-0.030494276369136,-0.240962440043193,
0.255690087090504));
#12405=CARTESIAN_POINT('Ctrl Pts',(-0.219014445044163,-0.105002353290262,
0.244573126782222));
#12406=CARTESIAN_POINT('Ctrl Pts',(-0.206963437784677,0.127117874085694,
0.233456166473939));
#12407=CARTESIAN_POINT('Ctrl Pts',(-0.00537745351023951,0.242824828130405,
0.222339206165656));
#12408=CARTESIAN_POINT('Ctrl Pts',(0.201133153391932,0.136155326051799,
0.211222245857373));
#12409=CARTESIAN_POINT('Ctrl Pts',(0.223448082612567,-0.0952038262864637,
0.20010528554909));
#12410=CARTESIAN_POINT('Ctrl Pts',(0.0411315804786337,-0.23937629702844,
0.188988325240808));
#12411=CARTESIAN_POINT('Ctrl Pts',(-0.178852833376126,-0.164330415102705,
0.177871364932525));
#12412=CARTESIAN_POINT('Ctrl Pts',(-0.235045601281728,0.0612075462746037,
0.166754404624242));
#12413=CARTESIAN_POINT('Ctrl Pts',(-0.0759861566816445,0.230692308120466,
0.155637444315959));
#12414=CARTESIAN_POINT('Ctrl Pts',(0.152660865452576,0.188911355652872,
0.144520484007676));
#12415=CARTESIAN_POINT('Ctrl Pts',(0.241502185356776,-0.0258725193599183,
0.133403523699394));
#12416=CARTESIAN_POINT('Ctrl Pts',(0.109179165064989,-0.216962892225182,
0.122286563391111));
#12417=CARTESIAN_POINT('Ctrl Pts',(-0.123130670689012,-0.209360343050761,
0.111169603082828));
#12418=CARTESIAN_POINT('Ctrl Pts',(-0.242675534991552,-0.0100287872532125,
0.100052642774545));
#12419=CARTESIAN_POINT('Ctrl Pts',(-0.139986704833514,0.198489007234759,
0.0889356824662626));
#12420=CARTESIAN_POINT('Ctrl Pts',(0.0909120711847139,0.225228838155139,
0.0778187221579794));
#12421=CARTESIAN_POINT('Ctrl Pts',(0.238532429865686,0.0457136341101189,
0.0667017618496969));
#12422=CARTESIAN_POINT('Ctrl Pts',(0.167749407629896,-0.175679414345444,
0.0555848015414138));
#12423=CARTESIAN_POINT('Ctrl Pts',(-0.056737317834033,-0.236160773940692,
0.0444678412331312));
#12424=CARTESIAN_POINT('Ctrl Pts',(-0.229110509130633,-0.0804187702998499,
0.0333508809248484));
#12425=CARTESIAN_POINT('Ctrl Pts',(-0.191963904396724,0.14906618911154,
0.0222339206165656));
#12426=CARTESIAN_POINT('Ctrl Pts',(0.0215757967252497,0.241850803896632,
0.0111169603082828));
#12427=CARTESIAN_POINT('Ctrl Pts',(0.149857277933222,0.156313104352978,
0.00370565343609428));
#12428=CARTESIAN_POINT('Ctrl Pts',(0.181742788875947,0.0958620587959227,
0.));
#12429=CARTESIAN_POINT('Ctrl Pts',(0.181742788875947,0.0958620587959227,
0.));
#12430=CARTESIAN_POINT('Ctrl Pts',(0.174504469275116,0.106933967990933,
1.09227492917999E-17));
#12431=CARTESIAN_POINT('Ctrl Pts',(0.166155260988786,0.117183932421154,
8.28421226973214E-17));
#12432=CARTESIAN_POINT('Ctrl Pts',(0.156880171408913,0.126533297038658,
1.45716771982052E-16));
#12433=CARTESIAN_POINT('Ctrl Pts',(0.152161070776583,0.131290188290046,
1.77706953278083E-16));
#12434=CARTESIAN_POINT('Ctrl Pts',(0.147201652193067,0.135813345993139,
6.21654697047341E-17));
#12435=CARTESIAN_POINT('Ctrl Pts',(0.142023529523608,0.140088211751239,
9.71445146547012E-17));
#12436=CARTESIAN_POINT('Ctrl Pts',(0.138407013399961,0.143073873143886,
1.21574658188656E-16));
#12437=CARTESIAN_POINT('Ctrl Pts',(0.134683780798487,0.145938358461697,
2.40181658122892E-17));
#12438=CARTESIAN_POINT('Ctrl Pts',(0.130860959346397,0.148675760328277,
3.46944695195361E-18));
#12439=CARTESIAN_POINT('Ctrl Pts',(0.127608826692069,0.151004509946822,
-1.40116623407028E-17));
#12440=CARTESIAN_POINT('Ctrl Pts',(0.124283670899528,0.153241554310962,
1.50905609184793E-16));
#12441=CARTESIAN_POINT('Ctrl Pts',(0.120904294225889,0.155374611387964,
1.45716771982052E-16));
#12442=CARTESIAN_POINT('Ctrl Pts',(0.109987742648693,0.162265121043141,
1.2895503914793E-16));
#12443=CARTESIAN_POINT('Ctrl Pts',(0.0984734851501926,0.168099067174435,
6.42435548254899E-17));
#12444=CARTESIAN_POINT('Ctrl Pts',(0.0865220202785484,0.172774083264826,
1.21430643318376E-16));
#12445=CARTESIAN_POINT('Ctrl Pts',(0.0785613376854963,0.175888037881495,
1.5952206263826E-16));
#12446=CARTESIAN_POINT('Ctrl Pts',(0.0704062138058044,0.178486876003788,
2.3171885042452E-16));
#12447=CARTESIAN_POINT('Ctrl Pts',(0.0621035437179694,0.180527190751547,
3.17454396103756E-16));
#12448=CARTESIAN_POINT('Ctrl Pts',(0.058507058441047,0.181410998234318,
3.5459264494205E-16));
#12449=CARTESIAN_POINT('Ctrl Pts',(0.0548830801400362,0.182189535865417,
2.01904242815308E-16));
#12450=CARTESIAN_POINT('Ctrl Pts',(0.0512492809662162,0.18285695898382,
2.04697370165263E-16));
#12451=CARTESIAN_POINT('Ctrl Pts',(0.0397135857002833,0.184975730368547,
2.13564306505654E-16));
#12452=CARTESIAN_POINT('Ctrl Pts',(0.028043543428156,0.185987354367647,
2.12494214757903E-16));
#12453=CARTESIAN_POINT('Ctrl Pts',(0.0163641619208267,0.185791435560747,
1.37043154602168E-16));
#12454=CARTESIAN_POINT('Ctrl Pts',(0.0073677207352634,0.185640522430431,
7.89876483687746E-17));
#12455=CARTESIAN_POINT('Ctrl Pts',(-0.00163453813548323,0.184771897471103,
1.62267606068596E-16));
#12456=CARTESIAN_POINT('Ctrl Pts',(-0.0105685044145391,0.183215538396018,
1.40512601554121E-16));
#12457=CARTESIAN_POINT('Ctrl Pts',(-0.0140598689340656,0.182607318408986,
1.32010817630666E-16));
#12458=CARTESIAN_POINT('Ctrl Pts',(-0.0175381431895957,0.181894183787698,
7.91699990801813E-17));
#12459=CARTESIAN_POINT('Ctrl Pts',(-0.0209886167262666,0.181080905311167,
7.63278329429795E-17));
#12460=CARTESIAN_POINT('Ctrl Pts',(-0.0323062471842877,0.178413333698454,
6.70054643755085E-17));
#12461=CARTESIAN_POINT('Ctrl Pts',(-0.0433589456433749,0.17466582100756,
6.12246176381618E-17));
#12462=CARTESIAN_POINT('Ctrl Pts',(-0.0539912114056113,0.169918461793345,
1.11889664200504E-16));
#12463=CARTESIAN_POINT('Ctrl Pts',(-0.0600125950487974,0.16722988423518,
1.40582859938265E-16));
#12464=CARTESIAN_POINT('Ctrl Pts',(-0.0658987875201912,0.164219919342787,
2.24249992830267E-17));
#12465=CARTESIAN_POINT('Ctrl Pts',(-0.0716172696707604,0.160898707475948,
4.33680868994202E-18));
#12466=CARTESIAN_POINT('Ctrl Pts',(-0.0760153027671363,0.158344393354502,
-9.57465571395114E-18));
#12467=CARTESIAN_POINT('Ctrl Pts',(-0.0803162508173771,0.155603868531732,
-1.48983259173674E-17));
#12468=CARTESIAN_POINT('Ctrl Pts',(-0.0844844353506574,0.152695748064502,
3.38271077815477E-17));
#12469=CARTESIAN_POINT('Ctrl Pts',(-0.0920276705150646,0.147432872489875,
1.22006362309274E-16));
#12470=CARTESIAN_POINT('Ctrl Pts',(-0.099152018847274,0.141614034257408,
8.85855526066679E-17));
#12471=CARTESIAN_POINT('Ctrl Pts',(-0.105766305686817,0.135269691928801,
6.85215773010839E-17));
#12472=CARTESIAN_POINT('Ctrl Pts',(-0.109162917311535,0.132011703966182,
5.82181941224795E-17));
#12473=CARTESIAN_POINT('Ctrl Pts',(-0.112424939305554,0.1286141740075,1.36999553352078E-16));
#12474=CARTESIAN_POINT('Ctrl Pts',(-0.115528518436688,0.125092942690589,
1.02348685082632E-16));
#12475=CARTESIAN_POINT('Ctrl Pts',(-0.121701328713853,0.118089450289423,
3.34304372375245E-17));
#12476=CARTESIAN_POINT('Ctrl Pts',(-0.127260382917516,0.110586827172589,
-2.01783277537669E-16));
#12477=CARTESIAN_POINT('Ctrl Pts',(-0.132096989238305,0.102614780608902,
-1.94343239418027E-16));
#12478=CARTESIAN_POINT('Ctrl Pts',(-0.13264315472071,0.101714550908896,
-1.94099397054962E-16));
#12479=CARTESIAN_POINT('Ctrl Pts',(-0.133180081100841,0.100808327459115,
-1.57928992210108E-16));
#12480=CARTESIAN_POINT('Ctrl Pts',(-0.13370774202371,0.0998962637199362,
-1.59594559789866E-16));
#12481=CARTESIAN_POINT('Ctrl Pts',(0.126907087985239,0.10793586530485,0.4));
#12482=CARTESIAN_POINT('Ctrl Pts',(0.135120918952682,0.100273232772223,
0.4));
#12483=CARTESIAN_POINT('Ctrl Pts',(0.142440334671421,0.0917705069751769,
0.4));
#12484=CARTESIAN_POINT('Ctrl Pts',(0.148860643047452,0.0826217448708272,
0.4));
#12485=CARTESIAN_POINT('Ctrl Pts',(0.153627635655713,0.0758289120703041,
0.4));
#12486=CARTESIAN_POINT('Ctrl Pts',(0.157898622411989,0.0686786359716775,
0.4));
#12487=CARTESIAN_POINT('Ctrl Pts',(0.161661540306914,0.0612359751068587,
0.4));
#12488=CARTESIAN_POINT('Ctrl Pts',(0.16388186285071,0.0568444076675918,
0.4));
#12489=CARTESIAN_POINT('Ctrl Pts',(0.165926693810491,0.0523458113179846,
0.4));
#12490=CARTESIAN_POINT('Ctrl Pts',(0.167781066520691,0.0477820314419273,
0.4));
#12491=CARTESIAN_POINT('Ctrl Pts',(0.172341633340749,0.0365580617608034,
0.4));
#12492=CARTESIAN_POINT('Ctrl Pts',(0.175769157493551,0.0249160193243555,
0.4));
#12493=CARTESIAN_POINT('Ctrl Pts',(0.178035263064282,0.013054133205507,
0.4));
#12494=CARTESIAN_POINT('Ctrl Pts',(0.179475094745571,0.00551736190307963,
0.4));
#12495=CARTESIAN_POINT('Ctrl Pts',(0.180445326972124,-0.00210904157496798,
0.4));
#12496=CARTESIAN_POINT('Ctrl Pts',(0.180929120151574,-0.00977934713136979,
0.4));
#12497=CARTESIAN_POINT('Ctrl Pts',(0.181154933194268,-0.0133595030939983,
0.4));
#12498=CARTESIAN_POINT('Ctrl Pts',(0.181274227458584,-0.0169457739644438,
0.4));
#12499=CARTESIAN_POINT('Ctrl Pts',(0.181285848432905,-0.020523365665851,
0.4));
#12500=CARTESIAN_POINT('Ctrl Pts',(0.181322136889233,-0.0316950003869775,
0.4));
#12501=CARTESIAN_POINT('Ctrl Pts',(0.180312890622882,-0.0428092364988491,
0.4));
#12502=CARTESIAN_POINT('Ctrl Pts',(0.178223999863926,-0.0537244994070254,
0.4));
#12503=CARTESIAN_POINT('Ctrl Pts',(0.177057515641768,-0.0598198310602051,
0.4));
#12504=CARTESIAN_POINT('Ctrl Pts',(0.175553812784148,-0.0658533566787336,
0.4));
#12505=CARTESIAN_POINT('Ctrl Pts',(0.173731861666353,-0.0718087245038544,
0.4));
#12506=CARTESIAN_POINT('Ctrl Pts',(0.172603795245643,-0.0754960080982815,
0.4));
#12507=CARTESIAN_POINT('Ctrl Pts',(0.171353052127964,-0.0791549057799955,
0.4));
#12508=CARTESIAN_POINT('Ctrl Pts',(0.169985341694702,-0.0827764782992071,
0.4));
#12509=CARTESIAN_POINT('Ctrl Pts',(0.165599957147556,-0.0943885767199536,
0.4));
#12510=CARTESIAN_POINT('Ctrl Pts',(0.16004703196815,-0.105538214993094,
0.4));
#12511=CARTESIAN_POINT('Ctrl Pts',(0.15349222199871,-0.116102682049509,
0.4));
#12512=CARTESIAN_POINT('Ctrl Pts',(0.14912551617891,-0.123140554999816,
0.4));
#12513=CARTESIAN_POINT('Ctrl Pts',(0.144312975580892,-0.129918879661908,
0.4));
#12514=CARTESIAN_POINT('Ctrl Pts',(0.139091822508928,-0.136399113069713,
0.4));
#12515=CARTESIAN_POINT('Ctrl Pts',(0.136383714422365,-0.139760281044032,
0.4));
#12516=CARTESIAN_POINT('Ctrl Pts',(0.133564151682456,-0.143042704899511,
0.4));
#12517=CARTESIAN_POINT('Ctrl Pts',(0.130641922795716,-0.146235745996435,
0.4));
#12518=CARTESIAN_POINT('Ctrl Pts',(0.124365895374187,-0.153093392765072,
0.4));
#12519=CARTESIAN_POINT('Ctrl Pts',(0.117640209417206,-0.159514676117615,
0.4));
#12520=CARTESIAN_POINT('Ctrl Pts',(0.110519094379635,-0.165448666244203,
0.4));
#12521=CARTESIAN_POINT('Ctrl Pts',(0.10626436178384,-0.16899411398399,0.4));
#12522=CARTESIAN_POINT('Ctrl Pts',(0.101868233565619,-0.172365528274035,
0.4));
#12523=CARTESIAN_POINT('Ctrl Pts',(0.0973404972469461,-0.175550904191779,
0.4));
#12524=CARTESIAN_POINT('Ctrl Pts',(0.0930576015741493,-0.178564028582011,
0.4));
#12525=CARTESIAN_POINT('Ctrl Pts',(0.0886627168583513,-0.181406366089281,
0.4));
#12526=CARTESIAN_POINT('Ctrl Pts',(0.0841711556372007,-0.184064773403165,
0.4));
#12527=CARTESIAN_POINT('Ctrl Pts',(0.0753868150238001,-0.189263935606354,
0.4));
#12528=CARTESIAN_POINT('Ctrl Pts',(0.066226257790498,-0.193765534094033,
0.4));
#12529=CARTESIAN_POINT('Ctrl Pts',(0.0567496916571122,-0.197494094154161,
0.4));
#12530=CARTESIAN_POINT('Ctrl Pts',(0.0555462198478251,-0.197967600787095,
0.4));
#12531=CARTESIAN_POINT('Ctrl Pts',(0.0543376370455851,-0.198428620952922,
0.4));
#12532=CARTESIAN_POINT('Ctrl Pts',(0.0531241180331689,-0.198877208092299,
0.4));
#12533=CARTESIAN_POINT('Ctrl Pts',(-0.166734374774229,-0.000128818837332453,
0.287148036339021));
#12534=CARTESIAN_POINT('Ctrl Pts',(-0.166805683280028,-0.00849491841283494,
0.287708823198405));
#12535=CARTESIAN_POINT('Ctrl Pts',(-0.166230437310337,-0.0168511701535723,
0.288269610057788));
#12536=CARTESIAN_POINT('Ctrl Pts',(-0.164974647650257,-0.0251038529149813,
0.288830396917172));
#12537=CARTESIAN_POINT('Ctrl Pts',(-0.156676448091865,-0.0796371960561269,
0.292536050353266));
#12538=CARTESIAN_POINT('Ctrl Pts',(-0.118662275502213,-0.12964819472467,
0.296241703789361));
#12539=CARTESIAN_POINT('Ctrl Pts',(-0.0683387086198173,-0.152238380008822,
0.299947357225455));
#12540=CARTESIAN_POINT('Ctrl Pts',(-0.0180151417374213,-0.174828565292974,
0.303653010661549));
#12541=CARTESIAN_POINT('Ctrl Pts',(0.0446178194377184,-0.169997937192735,
0.307358664097643));
#12542=CARTESIAN_POINT('Ctrl Pts',(0.0908810274585605,-0.139955915381198,
0.311064317533737));
#12543=CARTESIAN_POINT('Ctrl Pts',(0.137144235479403,-0.109913893569661,
0.314769970969832));
#12544=CARTESIAN_POINT('Ctrl Pts',(0.167037690345947,-0.0546604780468253,
0.318475624405926));
#12545=CARTESIAN_POINT('Ctrl Pts',(0.166873022942857,0.000499304166692509,
0.32218127784202));
#12546=CARTESIAN_POINT('Ctrl Pts',(0.166708355539768,0.0556590863802101,
0.325886931278115));
#12547=CARTESIAN_POINT('Ctrl Pts',(0.136485565867044,0.11072523528441,0.329592584714209));
#12548=CARTESIAN_POINT('Ctrl Pts',(0.0900441060064607,0.14049235813006,
0.333298238150303));
#12549=CARTESIAN_POINT('Ctrl Pts',(0.0436026461458773,0.17025948097571,
0.337003891586398));
#12550=CARTESIAN_POINT('Ctrl Pts',(-0.0190574839025661,0.17472757776281,
0.340709545022492));
#12551=CARTESIAN_POINT('Ctrl Pts',(-0.0692456664745192,0.151833326479749,
0.344415198458586));
#12552=CARTESIAN_POINT('Ctrl Pts',(-0.119433849046472,0.128939075196688,
0.34812085189468));
#12553=CARTESIAN_POINT('Ctrl Pts',(-0.157150084141935,0.0786824758434663,
0.351826505330774));
#12554=CARTESIAN_POINT('Ctrl Pts',(-0.165122125799463,0.0241090428979018,
0.355532158766869));
#12555=CARTESIAN_POINT('Ctrl Pts',(-0.166280881696888,0.0161766599544818,
0.356070784624253));
#12556=CARTESIAN_POINT('Ctrl Pts',(-0.166811221943148,0.00815307380534813,
0.356609410481637));
#12557=CARTESIAN_POINT('Ctrl Pts',(-0.166743774672904,0.000120896768023321,
0.357148036339021));
#12558=CARTESIAN_POINT('Ctrl Pts',(-0.0530170217188623,-0.198517432567172,
0.4));
#12559=CARTESIAN_POINT('Ctrl Pts',(-0.11904762702766,-0.180882981070921,
0.396294346563906));
#12560=CARTESIAN_POINT('Ctrl Pts',(-0.230986109789671,-0.0748521771817606,
0.388883039691718));
#12561=CARTESIAN_POINT('Ctrl Pts',(-0.188044707355364,0.153980890332211,
0.377766079383434));
#12562=CARTESIAN_POINT('Ctrl Pts',(0.0274206054315193,0.241260887402562,
0.366649119075152));
#12563=CARTESIAN_POINT('Ctrl Pts',(0.217614460633585,0.107865604001965,
0.355532158766869));
#12564=CARTESIAN_POINT('Ctrl Pts',(0.208602501412145,-0.124451281241526,
0.344415198458586));
#12565=CARTESIAN_POINT('Ctrl Pts',(0.00851095428263868,-0.242724098340208,
0.333298238150303));
#12566=CARTESIAN_POINT('Ctrl Pts',(-0.199352014072673,-0.138750852759731,
0.322181277842021));
#12567=CARTESIAN_POINT('Ctrl Pts',(-0.224662422339736,0.0923089884040401,
0.311064317533737));
#12568=CARTESIAN_POINT('Ctrl Pts',(-0.0442230349178335,0.238822732453524,
0.299947357225455));
#12569=CARTESIAN_POINT('Ctrl Pts',(0.176712068309585,0.166630571298318,
0.288830396917172));
#12570=CARTESIAN_POINT('Ctrl Pts',(0.235817802334529,-0.0581630255277868,
0.277713436608889));
#12571=CARTESIAN_POINT('Ctrl Pts',(0.078963123396891,-0.229690015875461,
0.266596476300606));
#12572=CARTESIAN_POINT('Ctrl Pts',(-0.150204697278654,-0.190870048415461,
0.255479515992324));
#12573=CARTESIAN_POINT('Ctrl Pts',(-0.241816852586086,0.0227471549627035,
0.24436255568404));
#12574=CARTESIAN_POINT('Ctrl Pts',(-0.111975498770539,0.215532531397883,
0.233245595375758));
#12575=CARTESIAN_POINT('Ctrl Pts',(0.120411794779082,0.210935552206459,
0.222128635067475));
#12576=CARTESIAN_POINT('Ctrl Pts',(0.242527242701154,0.0131659096813392,
0.211011674759192));
#12577=CARTESIAN_POINT('Ctrl Pts',(0.142538726865704,-0.196660905158453,
0.199894714450909));
#12578=CARTESIAN_POINT('Ctrl Pts',(-0.087985280286033,-0.226387709039377,
0.188777754142627));
#12579=CARTESIAN_POINT('Ctrl Pts',(-0.237933270688755,-0.0487909722550137,
0.177660793834344));
#12580=CARTESIAN_POINT('Ctrl Pts',(-0.169984441135179,0.173488023799692,
0.166543833526061));
#12581=CARTESIAN_POINT('Ctrl Pts',(0.0536344200204105,0.236888489580304,
0.155426873217778));
#12582=CARTESIAN_POINT('Ctrl Pts',(0.228135366692393,0.0833488984919273,
0.144309912909495));
#12583=CARTESIAN_POINT('Ctrl Pts',(0.193712423773769,-0.146520715699965,
0.133192952601213));
#12584=CARTESIAN_POINT('Ctrl Pts',(-0.0181106010581924,-0.24220824221319,
0.12207599229293));
#12585=CARTESIAN_POINT('Ctrl Pts',(-0.213347662204506,-0.116083820066942,
0.110959031984647));
#12586=CARTESIAN_POINT('Ctrl Pts',(-0.213204016359896,0.116348703664639,
0.0998420716763642));
#12587=CARTESIAN_POINT('Ctrl Pts',(-0.0178086481209368,0.24223078753445,
0.0887251113680815));
#12588=CARTESIAN_POINT('Ctrl Pts',(0.193892484656356,0.146279454291081,
0.0776081510597986));
#12589=CARTESIAN_POINT('Ctrl Pts',(0.228035008840565,-0.083631262664263,
0.0664911907515159));
#12590=CARTESIAN_POINT('Ctrl Pts',(0.0533337265757384,-0.236956827852518,
0.0553742304432329));
#12591=CARTESIAN_POINT('Ctrl Pts',(-0.170187709596901,-0.173273101663325,
0.0442572701349502));
#12592=CARTESIAN_POINT('Ctrl Pts',(-0.237895601007659,0.0490796089966686,
0.0331403098266674));
#12593=CARTESIAN_POINT('Ctrl Pts',(-0.0876598130547602,0.226510042114602,
0.0220233495183845));
#12594=CARTESIAN_POINT('Ctrl Pts',(0.142698384035228,0.196458332951895,
0.0109063892101018));
#12595=CARTESIAN_POINT('Ctrl Pts',(0.24267446543039,-0.0134175400107161,
-0.000210571098181212));
#12596=CARTESIAN_POINT('Ctrl Pts',(0.119815853924742,-0.211190891121989,
-0.0113275314064637));
#12597=CARTESIAN_POINT('Ctrl Pts',(-0.0343461939027931,-0.213802079752306,
-0.0187388382786524));
#12598=CARTESIAN_POINT('Ctrl Pts',(-0.0949553552261488,-0.182218155349229,
-0.0224444917147467));
#12599=CARTESIAN_POINT('Ctrl Pts',(-0.0496734897087706,-0.185997880000276,
0.407481497238249));
#12600=CARTESIAN_POINT('Ctrl Pts',(-0.111539858035973,-0.16947554968976,
0.403775843802155));
#12601=CARTESIAN_POINT('Ctrl Pts',(-0.216418911804395,-0.0701316055178259,
0.396364536929966));
#12602=CARTESIAN_POINT('Ctrl Pts',(-0.176185619877666,0.144270046171665,
0.385247576621683));
#12603=CARTESIAN_POINT('Ctrl Pts',(0.0256913179494246,0.226045707943951,
0.3741306163134));
#12604=CARTESIAN_POINT('Ctrl Pts',(0.203890549116156,0.101063032147195,
0.363013656005118));
#12605=CARTESIAN_POINT('Ctrl Pts',(0.195446931403795,-0.116602729417274,
0.351896695696835));
#12606=CARTESIAN_POINT('Ctrl Pts',(0.00797420877793362,-0.227416641110252,
0.340779735388552));
#12607=CARTESIAN_POINT('Ctrl Pts',(-0.186779828410061,-0.130000494806964,
0.329662775080269));
#12608=CARTESIAN_POINT('Ctrl Pts',(-0.210494029317946,0.0864874984836005,
0.318545814771986));
#12609=CARTESIAN_POINT('Ctrl Pts',(-0.0414340979304776,0.223761315859241,
0.307428854463704));
#12610=CARTESIAN_POINT('Ctrl Pts',(0.165567676606563,0.156121971778146,
0.29631189415542));
#12611=CARTESIAN_POINT('Ctrl Pts',(0.220945892425368,-0.0544949594736963,
0.285194933847139));
#12612=CARTESIAN_POINT('Ctrl Pts',(0.0739832938603632,-0.215204556383782,
0.274077973538855));
#12613=CARTESIAN_POINT('Ctrl Pts',(-0.140731999697103,-0.178832780082491,
0.262961013230573));
#12614=CARTESIAN_POINT('Ctrl Pts',(-0.226566611041236,0.0213125998275689,
0.251844052922289));
#12615=CARTESIAN_POINT('Ctrl Pts',(-0.104913735352921,0.201939917279227,
0.240727092614007));
#12616=CARTESIAN_POINT('Ctrl Pts',(0.112817994199877,0.197632847754131,
0.229610132305724));
#12617=CARTESIAN_POINT('Ctrl Pts',(0.227232200222333,0.0123355982259926,
0.218493171997441));
#12618=CARTESIAN_POINT('Ctrl Pts',(0.133549485665389,-0.184258434966565,
0.207376211689158));
#12619=CARTESIAN_POINT('Ctrl Pts',(-0.0824364661219098,-0.212110510371403,
0.196259251380876));
#12620=CARTESIAN_POINT('Ctrl Pts',(-0.22292794822775,-0.0457139571332818,
0.185142291072593));
#12621=CARTESIAN_POINT('Ctrl Pts',(-0.159264328957493,0.162546957286794,
0.17402533076431));
#12622=CARTESIAN_POINT('Ctrl Pts',(0.050251951628808,0.221949056506638,
0.162908370456027));
#12623=CARTESIAN_POINT('Ctrl Pts',(0.213747951548351,0.0780924789293308,
0.151791410147744));
#12624=CARTESIAN_POINT('Ctrl Pts',(0.181495900313161,-0.137280349357204,
0.140674449839462));
#12625=CARTESIAN_POINT('Ctrl Pts',(-0.0169684513787713,-0.226933317581584,
0.129557489531179));
#12626=CARTESIAN_POINT('Ctrl Pts',(-0.199892837419333,-0.108762964317901,
0.118440529222896));
#12627=CARTESIAN_POINT('Ctrl Pts',(-0.199758250636587,0.109011142963884,
0.107323568914613));
#12628=CARTESIAN_POINT('Ctrl Pts',(-0.0166855411805929,0.226954441076403,
0.0962066086063302));
#12629=CARTESIAN_POINT('Ctrl Pts',(0.181664605610217,0.137054303160666,
0.0850896482980475));
#12630=CARTESIAN_POINT('Ctrl Pts',(0.213653922790069,-0.0783570357330495,
0.0739726879897647));
#12631=CARTESIAN_POINT('Ctrl Pts',(0.0499702214929919,-0.222013085008269,
0.0628557276814818));
#12632=CARTESIAN_POINT('Ctrl Pts',(-0.159454778241781,-0.162345589269827,
0.0517387673731991));
#12633=CARTESIAN_POINT('Ctrl Pts',(-0.222892654194709,0.0459843909251343,
0.0406218070649163));
#12634=CARTESIAN_POINT('Ctrl Pts',(-0.0821315245646701,0.212225128480008,
0.0295048467566334));
#12635=CARTESIAN_POINT('Ctrl Pts',(0.133699074014756,0.18406863802793,0.0183878864483507));
#12636=CARTESIAN_POINT('Ctrl Pts',(0.227370138312564,-0.0125713594244052,
0.00727092614006769));
#12637=CARTESIAN_POINT('Ctrl Pts',(0.112259636507661,-0.197872083655765,
-0.00384603416821484));
#12638=CARTESIAN_POINT('Ctrl Pts',(-0.0321801424156356,-0.200318597008467,
-0.0112573410404035));
#12639=CARTESIAN_POINT('Ctrl Pts',(-0.0889669715064481,-0.170726520861333,
-0.0149629944764978));
#12640=CARTESIAN_POINT('Ctrl Pts',(-0.0463299576986789,-0.17347832743338,
0.414962994476498));
#12641=CARTESIAN_POINT('Ctrl Pts',(-0.104032089044287,-0.158068118308599,
0.411257341040404));
#12642=CARTESIAN_POINT('Ctrl Pts',(-0.201851713819119,-0.0654110338538912,
0.403846034168215));
#12643=CARTESIAN_POINT('Ctrl Pts',(-0.164326532399969,0.134559202011118,
0.392729073859932));
#12644=CARTESIAN_POINT('Ctrl Pts',(0.0239620304673297,0.210830528485339,
0.38161211355165));
#12645=CARTESIAN_POINT('Ctrl Pts',(0.190166637598728,0.0942604602924253,
0.370495153243366));
#12646=CARTESIAN_POINT('Ctrl Pts',(0.182291361395445,-0.108754177593023,
0.359378192935084));
#12647=CARTESIAN_POINT('Ctrl Pts',(0.00743746327322925,-0.212109183880296,
0.348261232626801));
#12648=CARTESIAN_POINT('Ctrl Pts',(-0.17420764274745,-0.121250136854196,
0.337144272318518));
#12649=CARTESIAN_POINT('Ctrl Pts',(-0.196325636296155,0.0806660085631606,
0.326027312010236));
#12650=CARTESIAN_POINT('Ctrl Pts',(-0.0386451609431219,0.208699899264959,
0.314910351701952));
#12651=CARTESIAN_POINT('Ctrl Pts',(0.154423284903542,0.145613372257974,
0.30379339139367));
#12652=CARTESIAN_POINT('Ctrl Pts',(0.206073982516206,-0.0508268934196057,
0.292676431085387));
#12653=CARTESIAN_POINT('Ctrl Pts',(0.0690034643238352,-0.200719096892102,
0.281559470777104));
#12654=CARTESIAN_POINT('Ctrl Pts',(-0.131259302115551,-0.166795511749521,
0.270442510468821));
#12655=CARTESIAN_POINT('Ctrl Pts',(-0.211316369496387,0.0198780446924348,
0.259325550160539));
#12656=CARTESIAN_POINT('Ctrl Pts',(-0.097851971935304,0.188347303160571,
0.248208589852256));
#12657=CARTESIAN_POINT('Ctrl Pts',(0.105224193620671,0.184330143301803,
0.237091629543973));
#12658=CARTESIAN_POINT('Ctrl Pts',(0.211937157743512,0.0115052867706461,
0.22597466923569));
#12659=CARTESIAN_POINT('Ctrl Pts',(0.124560244465074,-0.171855964774677,
0.214857708927407));
#12660=CARTESIAN_POINT('Ctrl Pts',(-0.0768876519577869,-0.197833311703429,
0.203740748619125));
#12661=CARTESIAN_POINT('Ctrl Pts',(-0.207922625766744,-0.0426369420115498,
0.192623788310841));
#12662=CARTESIAN_POINT('Ctrl Pts',(-0.148544216779807,0.151605890773896,
0.181506828002559));
#12663=CARTESIAN_POINT('Ctrl Pts',(0.0468694832372058,0.207009623432973,
0.170389867694276));
#12664=CARTESIAN_POINT('Ctrl Pts',(0.199360536404307,0.0728360593667339,
0.159272907385993));
#12665=CARTESIAN_POINT('Ctrl Pts',(0.169279376852553,-0.128039983014444,
0.148155947077711));
#12666=CARTESIAN_POINT('Ctrl Pts',(-0.0158263016993501,-0.211658392949978,
0.137038986769427));
#12667=CARTESIAN_POINT('Ctrl Pts',(-0.18643801263416,-0.101442108568861,
0.125922026461145));
#12668=CARTESIAN_POINT('Ctrl Pts',(-0.186312484913278,0.101673582263129,
0.114805066152862));
#12669=CARTESIAN_POINT('Ctrl Pts',(-0.0155624342402491,0.211678094618356,
0.103688105844579));
#12670=CARTESIAN_POINT('Ctrl Pts',(0.169436726564079,0.127829152030252,
0.0925711455362964));
#12671=CARTESIAN_POINT('Ctrl Pts',(0.199272836739573,-0.0730828088018361,
0.0814541852280136));
#12672=CARTESIAN_POINT('Ctrl Pts',(0.0466067164102457,-0.207069342164019,
0.0703372249197308));
#12673=CARTESIAN_POINT('Ctrl Pts',(-0.148721846886662,-0.15141807687633,
0.0592202646114479));
#12674=CARTESIAN_POINT('Ctrl Pts',(-0.207889707381759,0.0428891728536002,
0.0481033043031653));
#12675=CARTESIAN_POINT('Ctrl Pts',(-0.07660323607458,0.197940214845413,
0.0369863439948823));
#12676=CARTESIAN_POINT('Ctrl Pts',(0.124699763994284,0.171678943103966,
0.0258693836865997));
#12677=CARTESIAN_POINT('Ctrl Pts',(0.212065811194736,-0.0117251788380946,
0.0147524233783166));
#12678=CARTESIAN_POINT('Ctrl Pts',(0.10470341909058,-0.184553276189541,
0.00363546307003411));
#12679=CARTESIAN_POINT('Ctrl Pts',(-0.030014090928478,-0.186835114264629,
-0.00377584380215461));
#12680=CARTESIAN_POINT('Ctrl Pts',(-0.0829785877867473,-0.159234886373437,
-0.00748149723824889));
#12681=CARTESIAN_POINT('Ctrl Pts',(-0.0429864256885872,-0.160958774866484,
0.422444491714747));
#12682=CARTESIAN_POINT('Ctrl Pts',(-0.0965243200526006,-0.146660686927438,
0.418738838278652));
#12683=CARTESIAN_POINT('Ctrl Pts',(-0.187284515833844,-0.0606904621899564,
0.411327531406464));
#12684=CARTESIAN_POINT('Ctrl Pts',(-0.152467444922271,0.124848357850572,
0.400210571098181));
#12685=CARTESIAN_POINT('Ctrl Pts',(0.0222327429852349,0.195615349026728,
0.389093610789898));
#12686=CARTESIAN_POINT('Ctrl Pts',(0.1764427260813,0.0874578884376555,0.377976650481615));
#12687=CARTESIAN_POINT('Ctrl Pts',(0.169135791387095,-0.100905625768771,
0.366859690173333));
#12688=CARTESIAN_POINT('Ctrl Pts',(0.00690071776852435,-0.19680172665034,
0.35574272986505));
#12689=CARTESIAN_POINT('Ctrl Pts',(-0.161635457084839,-0.112499778901429,
0.344625769556767));
#12690=CARTESIAN_POINT('Ctrl Pts',(-0.182157243274365,0.0748445186427209,
0.333508809248484));
#12691=CARTESIAN_POINT('Ctrl Pts',(-0.035856223955766,0.193638482670676,
0.322391848940201));
#12692=CARTESIAN_POINT('Ctrl Pts',(0.14327889320052,0.135104772737801,0.311274888631918));
#12693=CARTESIAN_POINT('Ctrl Pts',(0.191202072607045,-0.0471588273655153,
0.300157928323636));
#12694=CARTESIAN_POINT('Ctrl Pts',(0.0640236347873075,-0.186233637400423,
0.289040968015352));
#12695=CARTESIAN_POINT('Ctrl Pts',(-0.121786604534,-0.154758243416551,0.277924007707071));
#12696=CARTESIAN_POINT('Ctrl Pts',(-0.196066127951537,0.0184434895573008,
0.266807047398787));
#12697=CARTESIAN_POINT('Ctrl Pts',(-0.090790208517687,0.174754689041914,
0.255690087090505));
#12698=CARTESIAN_POINT('Ctrl Pts',(0.0976303930414654,0.171027438849476,
0.244573126782221));
#12699=CARTESIAN_POINT('Ctrl Pts',(0.196642115264691,0.0106749753152992,
0.233456166473939));
#12700=CARTESIAN_POINT('Ctrl Pts',(0.115571003264759,-0.159453494582788,
0.222339206165656));
#12701=CARTESIAN_POINT('Ctrl Pts',(-0.0713388377936639,-0.183556113035455,
0.211222245857374));
#12702=CARTESIAN_POINT('Ctrl Pts',(-0.192917303305739,-0.0395599268898177,
0.20010528554909));
#12703=CARTESIAN_POINT('Ctrl Pts',(-0.137824104602121,0.140664824260998,
0.188988325240808));
#12704=CARTESIAN_POINT('Ctrl Pts',(0.0434870148456035,0.192070190359307,
0.177871364932525));
#12705=CARTESIAN_POINT('Ctrl Pts',(0.184973121260264,0.0675796398041375,
0.166754404624242));
#12706=CARTESIAN_POINT('Ctrl Pts',(0.157062853391945,-0.118799616671684,
0.155637444315959));
#12707=CARTESIAN_POINT('Ctrl Pts',(-0.0146841520199287,-0.196383468318372,
0.144520484007676));
#12708=CARTESIAN_POINT('Ctrl Pts',(-0.172983187848988,-0.0941212528198204,
0.133403523699394));
#12709=CARTESIAN_POINT('Ctrl Pts',(-0.172866719189968,0.0943360215623745,
0.122286563391111));
#12710=CARTESIAN_POINT('Ctrl Pts',(-0.0144393272999055,0.196401748160308,
0.111169603082828));
#12711=CARTESIAN_POINT('Ctrl Pts',(0.157208847517941,0.118604000899837,
0.100052642774545));
#12712=CARTESIAN_POINT('Ctrl Pts',(0.184891750689077,-0.0678085818706227,
0.0889356824662626));
#12713=CARTESIAN_POINT('Ctrl Pts',(0.0432432113274997,-0.192125599319769,
0.0778187221579795));
#12714=CARTESIAN_POINT('Ctrl Pts',(-0.137988915531543,-0.140490564482832,
0.0667017618496969));
#12715=CARTESIAN_POINT('Ctrl Pts',(-0.192886760568809,0.039793954782066,
0.0555848015414141));
#12716=CARTESIAN_POINT('Ctrl Pts',(-0.0710749475844899,0.183655301210818,
0.0444678412331312));
#12717=CARTESIAN_POINT('Ctrl Pts',(0.115700453973812,0.159289248180001,
0.0333508809248486));
#12718=CARTESIAN_POINT('Ctrl Pts',(0.19676148407691,-0.0108789982517839,
0.0222339206165655));
#12719=CARTESIAN_POINT('Ctrl Pts',(0.0971472016734982,-0.171234468723317,
0.011116960308283));
#12720=CARTESIAN_POINT('Ctrl Pts',(-0.0278480394413205,-0.17335163152079,
0.00370565343609428));
#12721=CARTESIAN_POINT('Ctrl Pts',(-0.0769902040670466,-0.147743251885541,
0.));
#12722=CARTESIAN_POINT('Ctrl Pts',(-0.0769902040670466,-0.147743251885541,
0.));
#12723=CARTESIAN_POINT('Ctrl Pts',(-0.0676919232950484,-0.154046060403006,
-1.40302012364989E-17));
#12724=CARTESIAN_POINT('Ctrl Pts',(-0.0577736401959485,-0.159289942754579,
-5.08211119036949E-18));
#12725=CARTESIAN_POINT('Ctrl Pts',(-0.0474255897387057,-0.163513503780882,
-6.24500451351651E-17));
#12726=CARTESIAN_POINT('Ctrl Pts',(-0.0397423269274568,-0.16664943063962,
-1.05044823277914E-16));
#12727=CARTESIAN_POINT('Ctrl Pts',(-0.0318209566230111,-0.169222252731152,
-2.46304152627642E-17));
#12728=CARTESIAN_POINT('Ctrl Pts',(-0.0237275895471058,-0.17123468536678,
-2.77555756156289E-17));
#12729=CARTESIAN_POINT('Ctrl Pts',(-0.0189520706408748,-0.172422128121918,
-2.9599587163621E-17));
#12730=CARTESIAN_POINT('Ctrl Pts',(-0.0141112573217385,-0.17341466403244,
-4.4351679547558E-17));
#12731=CARTESIAN_POINT('Ctrl Pts',(-0.00924927591576842,-0.174207012929982,
-2.77555756156289E-17));
#12732=CARTESIAN_POINT('Ctrl Pts',(0.00270810149489128,-0.176155686529844,
1.30602691378976E-17));
#12733=CARTESIAN_POINT('Ctrl Pts',(0.0148209433822563,-0.176906695131537,
1.46993562916598E-16));
#12734=CARTESIAN_POINT('Ctrl Pts',(0.0268896779998609,-0.176476481527875,
2.70616862252382E-16));
#12735=CARTESIAN_POINT('Ctrl Pts',(0.0345578784611946,-0.176203133554073,
3.49164304965678E-16));
#12736=CARTESIAN_POINT('Ctrl Pts',(0.0422089684879974,-0.175452013432818,
9.66603464943305E-17));
#12737=CARTESIAN_POINT('Ctrl Pts',(0.0497946177189777,-0.174216878926306,
8.32667268468867E-17));
#12738=CARTESIAN_POINT('Ctrl Pts',(0.0533352666340748,-0.173640372220377,
7.70151716497034E-17));
#12739=CARTESIAN_POINT('Ctrl Pts',(0.0568581744479369,-0.172958655817438,
1.70258089114663E-16));
#12740=CARTESIAN_POINT('Ctrl Pts',(0.060348661217807,-0.172173896054275,
1.78676518025611E-16));
#12741=CARTESIAN_POINT('Ctrl Pts',(0.0712482444786328,-0.169723362663869,
2.04964360636066E-16));
#12742=CARTESIAN_POINT('Ctrl Pts',(0.0818592181722872,-0.166266280890076,
6.45230284175388E-17));
#12743=CARTESIAN_POINT('Ctrl Pts',(0.0920359693799999,-0.161800897340594,
8.32667268468867E-17));
#12744=CARTESIAN_POINT('Ctrl Pts',(0.0977189075830844,-0.15930732171446,
9.2085789653526E-17));
#12745=CARTESIAN_POINT('Ctrl Pts',(0.103266552483982,-0.156498733846781,
1.36090193073051E-16));
#12746=CARTESIAN_POINT('Ctrl Pts',(0.10866718341613,-0.153397267387788,
1.35308431126191E-16));
#12747=CARTESIAN_POINT('Ctrl Pts',(0.11201100284804,-0.151476983638854,
1.34824400496829E-16));
#12748=CARTESIAN_POINT('Ctrl Pts',(0.115299850264095,-0.149443414758961,
6.72250876644913E-17));
#12749=CARTESIAN_POINT('Ctrl Pts',(0.118526280975827,-0.147304116216612,
7.45931094670027E-17));
#12750=CARTESIAN_POINT('Ctrl Pts',(0.128871394179061,-0.140444745111681,
9.82176737118538E-17));
#12751=CARTESIAN_POINT('Ctrl Pts',(0.138505844759193,-0.132550010250448,
1.65756112205145E-16));
#12752=CARTESIAN_POINT('Ctrl Pts',(0.147346858840741,-0.123808721893542,
1.51788304147971E-16));
#12753=CARTESIAN_POINT('Ctrl Pts',(0.153236584111842,-0.117985432114476,
1.42483200532319E-16));
#12754=CARTESIAN_POINT('Ctrl Pts',(0.158774063957949,-0.111785241608361,
1.64345680573043E-16));
#12755=CARTESIAN_POINT('Ctrl Pts',(0.163930004359885,-0.10525301636718,
1.83013326715553E-16));
#12756=CARTESIAN_POINT('Ctrl Pts',(0.166604294556271,-0.101864872874187,
1.92695886864967E-16));
#12757=CARTESIAN_POINT('Ctrl Pts',(0.169177014089436,-0.0983855914277328,
9.88896432374603E-17));
#12758=CARTESIAN_POINT('Ctrl Pts',(0.171639746961675,-0.0948261071091421,
6.33174068731535E-17));
#12759=CARTESIAN_POINT('Ctrl Pts',(0.176928913626705,-0.087181467280431,
-1.30804391537608E-17));
#12760=CARTESIAN_POINT('Ctrl Pts',(0.181692601485159,-0.0791955439239232,
1.01225052450567E-16));
#12761=CARTESIAN_POINT('Ctrl Pts',(0.185893224525176,-0.0709325403972633,
7.80625564189563E-17));
#12762=CARTESIAN_POINT('Ctrl Pts',(0.188402594077904,-0.065996384673136,
6.42257370345008E-17));
#12763=CARTESIAN_POINT('Ctrl Pts',(0.190710898758921,-0.0609611385701718,
-2.50862304223578E-17));
#12764=CARTESIAN_POINT('Ctrl Pts',(0.192808617454456,-0.0558390095854279,
8.67361737988404E-19));
#12765=CARTESIAN_POINT('Ctrl Pts',(0.194793596006727,-0.0509921651546984,
2.54260997148077E-17));
#12766=CARTESIAN_POINT('Ctrl Pts',(0.196587084810493,-0.0460741094242064,
1.76166452828751E-16));
#12767=CARTESIAN_POINT('Ctrl Pts',(0.198179668914476,-0.0411027133746267,
1.06251812903579E-16));
#12768=CARTESIAN_POINT('Ctrl Pts',(0.201293818615582,-0.0313816120003518,
-3.0459745676829E-17));
#12769=CARTESIAN_POINT('Ctrl Pts',(0.203644165628124,-0.0214489479791743,
-7.88851781500756E-17));
#12770=CARTESIAN_POINT('Ctrl Pts',(0.205170522984607,-0.0113802171361653,
-8.38359329874416E-17));
#12771=CARTESIAN_POINT('Ctrl Pts',(0.205364360570336,-0.0101015529559362,
-8.50972051141002E-17));
#12772=CARTESIAN_POINT('Ctrl Pts',(0.205544887409679,-0.00882068448784814,
-9.83390714117784E-17));
#12773=CARTESIAN_POINT('Ctrl Pts',(0.205712194497466,-0.00753777023904148,
-9.71445146547012E-17));
#12774=CARTESIAN_POINT('Ctrl Pts',(-0.166378928688253,9.26016813348553E-5,
0.337851963660979));
#12775=CARTESIAN_POINT('Ctrl Pts',(-0.166489498819458,0.0218084776863281,
0.336404245523481));
#12776=CARTESIAN_POINT('Ctrl Pts',(-0.162543310453018,0.0434858705291553,
0.334956527385983));
#12777=CARTESIAN_POINT('Ctrl Pts',(-0.154353442356344,0.0634194630566879,
0.333508809248484));
#12778=CARTESIAN_POINT('Ctrl Pts',(-0.133390236834832,0.114442506652039,
0.32980315581239));
#12779=CARTESIAN_POINT('Ctrl Pts',(-0.0846232303952993,0.154040494661357,
0.326097502376296));
#12780=CARTESIAN_POINT('Ctrl Pts',(-0.0303838743161517,0.164083870343871,
0.322391848940201));
#12781=CARTESIAN_POINT('Ctrl Pts',(0.0238554817629959,0.174127246026385,
0.318686195504107));
#12782=CARTESIAN_POINT('Ctrl Pts',(0.083567187481758,0.154616009382093,
0.314980542068013));
#12783=CARTESIAN_POINT('Ctrl Pts',(0.121410236908893,0.114483124376061,
0.311274888631919));
#12784=CARTESIAN_POINT('Ctrl Pts',(0.159253286336028,0.0743502393700291,
0.307569235195824));
#12785=CARTESIAN_POINT('Ctrl Pts',(0.175227679471537,0.0135957060022568,
0.30386358175973));
#12786=CARTESIAN_POINT('Ctrl Pts',(0.162018469736001,-0.0399606956874471,
0.300157928323636));
#12787=CARTESIAN_POINT('Ctrl Pts',(0.148809260000466,-0.0935170973771512,
0.296452274887542));
#12788=CARTESIAN_POINT('Ctrl Pts',(0.106416447393887,-0.139875367388787,
0.292746621451447));
#12789=CARTESIAN_POINT('Ctrl Pts',(0.0542516678703787,-0.157808603397293,
0.289040968015353));
#12790=CARTESIAN_POINT('Ctrl Pts',(0.00208688834687113,-0.175741839405799,
0.285335314579258));
#12791=CARTESIAN_POINT('Ctrl Pts',(-0.0598498580935646,-0.165250041411175,
0.281629661143165));
#12792=CARTESIAN_POINT('Ctrl Pts',(-0.103198151883372,-0.131137186918221,
0.27792400770707));
#12793=CARTESIAN_POINT('Ctrl Pts',(-0.142472010228314,-0.100230701380539,
0.274566659691707));
#12794=CARTESIAN_POINT('Ctrl Pts',(-0.166487561106675,-0.0499349019762822,
0.271209311676343));
#12795=CARTESIAN_POINT('Ctrl Pts',(-0.166813199754551,8.97901853038408E-5,
0.267851963660979));
#12796=CARTESIAN_POINT('Ctrl Pts',(-0.0530170217188623,-0.198517432567172,
0.4));
#12797=CARTESIAN_POINT('Ctrl Pts',(-0.0654220238783876,-0.193924320176499,
0.4));
#12798=CARTESIAN_POINT('Ctrl Pts',(-0.077272885559963,-0.188065277791306,
0.4));
#12799=CARTESIAN_POINT('Ctrl Pts',(-0.088451754807208,-0.181103168839745,
0.4));
#12800=CARTESIAN_POINT('Ctrl Pts',(-0.0941395501466508,-0.177560856109221,
0.4));
#12801=CARTESIAN_POINT('Ctrl Pts',(-0.0996529437908355,-0.17373223440453,
0.4));
#12802=CARTESIAN_POINT('Ctrl Pts',(-0.104972932012442,-0.169635136338519,
0.4));
#12803=CARTESIAN_POINT('Ctrl Pts',(-0.108688724528218,-0.166773482196456,
0.4));
#12804=CARTESIAN_POINT('Ctrl Pts',(-0.112310113490456,-0.163780806587061,
0.4));
#12805=CARTESIAN_POINT('Ctrl Pts',(-0.115829752094829,-0.160662744842601,
0.4));
#12806=CARTESIAN_POINT('Ctrl Pts',(-0.118823489359745,-0.158010581172415,
0.4));
#12807=CARTESIAN_POINT('Ctrl Pts',(-0.121744082040539,-0.15526683742813,
0.4));
#12808=CARTESIAN_POINT('Ctrl Pts',(-0.124575376453565,-0.152447107362845,
0.4));
#12809=CARTESIAN_POINT('Ctrl Pts',(-0.13372228318865,-0.14333756092832,
0.4));
#12810=CARTESIAN_POINT('Ctrl Pts',(-0.141972119474717,-0.133410188786047,
0.4));
#12811=CARTESIAN_POINT('Ctrl Pts',(-0.14918937059335,-0.122798683211669,
0.4));
#12812=CARTESIAN_POINT('Ctrl Pts',(-0.153996665370339,-0.115730530187037,
0.4));
#12813=CARTESIAN_POINT('Ctrl Pts',(-0.158345026572386,-0.108358186354888,
0.4));
#12814=CARTESIAN_POINT('Ctrl Pts',(-0.162181700444826,-0.100717710946895,
0.4));
#12815=CARTESIAN_POINT('Ctrl Pts',(-0.163843640896044,-0.0974080694268549,
0.4));
#12816=CARTESIAN_POINT('Ctrl Pts',(-0.165409068660182,-0.0940481991896131,
0.4));
#12817=CARTESIAN_POINT('Ctrl Pts',(-0.16686835322227,-0.0906540285733807,
0.4));
#12818=CARTESIAN_POINT('Ctrl Pts',(-0.171500933618561,-0.0798790442646778,
0.4));
#12819=CARTESIAN_POINT('Ctrl Pts',(-0.175084020385089,-0.0687267134060537,
0.4));
#12820=CARTESIAN_POINT('Ctrl Pts',(-0.177491918105115,-0.0572965665658765,
0.4));
#12821=CARTESIAN_POINT('Ctrl Pts',(-0.179346683049952,-0.0484921080138423,
0.4));
#12822=CARTESIAN_POINT('Ctrl Pts',(-0.180503025417496,-0.0395222674034557,
0.4));
#12823=CARTESIAN_POINT('Ctrl Pts',(-0.180973680426704,-0.0304659686022641,
0.4));
#12824=CARTESIAN_POINT('Ctrl Pts',(-0.181157610795637,-0.0269267979845529,
0.4));
#12825=CARTESIAN_POINT('Ctrl Pts',(-0.181236344221217,-0.0233770431725763,
0.4));
#12826=CARTESIAN_POINT('Ctrl Pts',(-0.181211258491791,-0.0198321075205306,
0.4));
#12827=CARTESIAN_POINT('Ctrl Pts',(-0.181128976637152,-0.00820462501560692,
0.4));
#12828=CARTESIAN_POINT('Ctrl Pts',(-0.179934875816279,0.00340488210138015,
0.4));
#12829=CARTESIAN_POINT('Ctrl Pts',(-0.177672440840337,0.0148269863576212,
0.4));
#12830=CARTESIAN_POINT('Ctrl Pts',(-0.176391160190413,0.0212956457094027,
0.4));
#12831=CARTESIAN_POINT('Ctrl Pts',(-0.174766470591578,0.0277040200840655,
0.4));
#12832=CARTESIAN_POINT('Ctrl Pts',(-0.172801022035689,0.0340181492506376,
0.4));
#12833=CARTESIAN_POINT('Ctrl Pts',(-0.171289396872808,0.0388743417473916,
0.4));
#12834=CARTESIAN_POINT('Ctrl Pts',(-0.169574623865183,0.0436773188170338,
0.4));
#12835=CARTESIAN_POINT('Ctrl Pts',(-0.167666912323756,0.0483881533931519,
0.4));
#12836=CARTESIAN_POINT('Ctrl Pts',(-0.164214525512166,0.0569133537753892,
0.4));
#12837=CARTESIAN_POINT('Ctrl Pts',(-0.160126908536967,0.0651538844249133,
0.4));
#12838=CARTESIAN_POINT('Ctrl Pts',(-0.15541346823496,0.0730140785601572,
0.4));
#12839=CARTESIAN_POINT('Ctrl Pts',(-0.152992964434853,0.0770505420676795,
0.4));
#12840=CARTESIAN_POINT('Ctrl Pts',(-0.150406465661651,0.0809868395219411,
0.4));
#12841=CARTESIAN_POINT('Ctrl Pts',(-0.147664107811223,0.0847961900136081,
0.4));
#12842=CARTESIAN_POINT('Ctrl Pts',(-0.142209781496364,0.092372677752427,
0.4));
#12843=CARTESIAN_POINT('Ctrl Pts',(-0.13613226485763,0.0994618610044957,
0.4));
#12844=CARTESIAN_POINT('Ctrl Pts',(-0.129436334451722,0.105951160758884,
0.4));
#12845=CARTESIAN_POINT('Ctrl Pts',(-0.128680208499678,0.106683953314577,
0.4));
#12846=CARTESIAN_POINT('Ctrl Pts',(-0.127916183191217,0.107409072087309,
0.4));
#12847=CARTESIAN_POINT('Ctrl Pts',(-0.127144402274346,0.108126457236474,
0.4));
#12848=CARTESIAN_POINT('Origin',(0.,0.,0.4));
#12849=CARTESIAN_POINT('',(0.202072594216369,-0.35,0.4));
#12850=CARTESIAN_POINT('',(0.404145188432738,0.,0.4));
#12851=CARTESIAN_POINT('',(0.202072594216369,-0.35,0.4));
#12852=CARTESIAN_POINT('',(0.202072594216369,0.35,0.4));
#12853=CARTESIAN_POINT('',(0.404145188432738,0.,0.4));
#12854=CARTESIAN_POINT('',(-0.202072594216369,0.35,0.4));
#12855=CARTESIAN_POINT('',(0.202072594216369,0.35,0.4));
#12856=CARTESIAN_POINT('',(-0.404145188432738,5.55111512312578E-17,0.4));
#12857=CARTESIAN_POINT('',(-0.202072594216369,0.35,0.4));
#12858=CARTESIAN_POINT('',(-0.202072594216369,-0.35,0.4));
#12859=CARTESIAN_POINT('',(-0.404145188432738,4.94935111404957E-17,0.4));
#12860=CARTESIAN_POINT('',(-0.202072594216369,-0.35,0.4));
#12861=CARTESIAN_POINT('Origin',(0.,0.,0.2));
#12862=CARTESIAN_POINT('Origin',(-0.202072594216369,-0.35,0.));
#12863=CARTESIAN_POINT('',(-0.202072594216369,-0.35,0.));
#12864=CARTESIAN_POINT('',(0.202072594216369,-0.35,0.));
#12865=CARTESIAN_POINT('',(-0.202072594216369,-0.35,0.));
#12866=CARTESIAN_POINT('',(0.202072594216369,-0.35,0.));
#12867=CARTESIAN_POINT('',(-0.202072594216369,-0.35,0.));
#12868=CARTESIAN_POINT('Origin',(-0.404145188432738,4.94935111404957E-17,
0.));
#12869=CARTESIAN_POINT('',(-0.404145188432738,4.94935111404957E-17,0.));
#12870=CARTESIAN_POINT('',(-0.404145188432738,4.94935111404957E-17,0.));
#12871=CARTESIAN_POINT('',(-0.404145188432738,4.94935111404957E-17,0.));
#12872=CARTESIAN_POINT('Origin',(-0.202072594216369,0.35,0.));
#12873=CARTESIAN_POINT('',(-0.202072594216369,0.35,0.));
#12874=CARTESIAN_POINT('',(-0.202072594216369,0.35,0.));
#12875=CARTESIAN_POINT('',(-0.202072594216369,0.35,0.));
#12876=CARTESIAN_POINT('Origin',(0.202072594216369,0.35,0.));
#12877=CARTESIAN_POINT('',(0.202072594216369,0.35,0.));
#12878=CARTESIAN_POINT('',(0.202072594216369,0.35,0.));
#12879=CARTESIAN_POINT('',(0.202072594216369,0.35,0.));
#12880=CARTESIAN_POINT('Origin',(0.404145188432738,0.,0.));
#12881=CARTESIAN_POINT('',(0.404145188432738,0.,0.));
#12882=CARTESIAN_POINT('',(0.404145188432738,0.,0.));
#12883=CARTESIAN_POINT('',(0.404145188432738,0.,0.));
#12884=CARTESIAN_POINT('Origin',(0.202072594216369,-0.35,0.));
#12885=CARTESIAN_POINT('',(0.202072594216369,-0.35,0.));
#12886=CARTESIAN_POINT('Origin',(0.,0.,0.));
#12887=CARTESIAN_POINT('',(0.,0.,0.));
#12888=CARTESIAN_POINT('Origin',(0.,0.,0.));
#12889=CARTESIAN_POINT('',(-0.4,-4.89858719658941E-17,2.8));
#12890=CARTESIAN_POINT('Origin',(0.,0.,2.8));
#12891=CARTESIAN_POINT('',(-0.4,-4.89858719658941E-17,0.));
#12892=CARTESIAN_POINT('',(-0.4,-4.89858719658941E-17,0.));
#12893=CARTESIAN_POINT('Origin',(0.,0.,0.));
#12894=CARTESIAN_POINT('Origin',(0.,0.,2.8));
#12895=CARTESIAN_POINT('Origin',(0.,0.,0.));
#12896=CARTESIAN_POINT('',(0.,0.,0.));
#12897=CARTESIAN_POINT('',(60.,0.,180.));
#12898=CARTESIAN_POINT('',(1.32,0.,0.));
#12899=CARTESIAN_POINT('',(1.32,58.2,1.32));
#12900=CARTESIAN_POINT('',(1.32,0.,89.1));
#12901=CARTESIAN_POINT('',(0.,0.,0.));
#12902=CARTESIAN_POINT('',(1.8,-0.4,5.));
#12903=CARTESIAN_POINT('',(1.8,-0.4,5.));
#12904=CARTESIAN_POINT('',(1.8,-0.4,5.));
#12905=CARTESIAN_POINT('',(2.,1.6,60.));
#12906=CARTESIAN_POINT('',(0.,1.6,60.));
#12907=CARTESIAN_POINT('',(58.6,9.,60.));
#12908=CARTESIAN_POINT('',(58.68,0.,180.));
#12909=CARTESIAN_POINT('',(3.4,1.77635683940025E-15,60.));
#12910=CARTESIAN_POINT('',(3.4,-2.,60.));
#12911=CARTESIAN_POINT('',(2.,1.6,120.));
#12912=CARTESIAN_POINT('',(0.,1.6,120.));
#12913=CARTESIAN_POINT('',(3.4,2.22044604925031E-15,120.));
#12914=CARTESIAN_POINT('',(3.4,-2.,120.));
#12915=CARTESIAN_POINT('',(60.,0.,0.));
#12916=CARTESIAN_POINT('',(120.,0.,180.));
#12917=CARTESIAN_POINT('',(61.32,0.,0.));
#12918=CARTESIAN_POINT('',(118.68,0.,180.));
#12919=CARTESIAN_POINT('',(61.32,58.2,1.32));
#12920=CARTESIAN_POINT('',(61.32,0.,89.1));
#12921=CARTESIAN_POINT('',(60.,0.,0.));
#12922=CARTESIAN_POINT('',(61.8,-0.4,5.));
#12923=CARTESIAN_POINT('',(61.8,-0.4,5.));
#12924=CARTESIAN_POINT('',(61.8,-0.4,5.));
#12925=CARTESIAN_POINT('',(62.,1.6,60.));
#12926=CARTESIAN_POINT('',(60.,1.6,60.));
#12927=CARTESIAN_POINT('',(63.4,1.77635683940025E-15,60.));
#12928=CARTESIAN_POINT('',(63.4,-2.,60.));
#12929=CARTESIAN_POINT('',(62.,1.6,120.));
#12930=CARTESIAN_POINT('',(60.,1.6,120.));
#12931=CARTESIAN_POINT('',(63.4,2.22044604925031E-15,120.));
#12932=CARTESIAN_POINT('',(63.4,-2.,120.));
#12933=CARTESIAN_POINT('',(58.6,9.,120.));
#12934=CARTESIAN_POINT('',(58.6,51.,60.));
#12935=CARTESIAN_POINT('',(58.6,51.,120.));
#12936=UNCERTAINTY_MEASURE_WITH_UNIT(LENGTH_MEASURE(0.001),#12964,
'DISTANCE_ACCURACY_VALUE',
'Maximum model space distance between geometric entities at asserted c
onnectivities');
#12937=UNCERTAINTY_MEASURE_WITH_UNIT(LENGTH_MEASURE(0.001),#12964,
'DISTANCE_ACCURACY_VALUE',
'Maximum model space distance between geometric entities at asserted c
onnectivities');
#12938=UNCERTAINTY_MEASURE_WITH_UNIT(LENGTH_MEASURE(0.001),#12964,
'DISTANCE_ACCURACY_VALUE',
'Maximum model space distance between geometric entities at asserted c
onnectivities');
#12939=UNCERTAINTY_MEASURE_WITH_UNIT(LENGTH_MEASURE(0.001),#12964,
'DISTANCE_ACCURACY_VALUE',
'Maximum model space distance between geometric entities at asserted c
onnectivities');
#12940=UNCERTAINTY_MEASURE_WITH_UNIT(LENGTH_MEASURE(0.001),#12964,
'DISTANCE_ACCURACY_VALUE',
'Maximum model space distance between geometric entities at asserted c
onnectivities');
#12941=UNCERTAINTY_MEASURE_WITH_UNIT(LENGTH_MEASURE(0.001),#12964,
'DISTANCE_ACCURACY_VALUE',
'Maximum model space distance between geometric entities at asserted c
onnectivities');
#12942=UNCERTAINTY_MEASURE_WITH_UNIT(LENGTH_MEASURE(0.001),#12964,
'DISTANCE_ACCURACY_VALUE',
'Maximum model space distance between geometric entities at asserted c
onnectivities');
#12943=UNCERTAINTY_MEASURE_WITH_UNIT(LENGTH_MEASURE(0.001),#12964,
'DISTANCE_ACCURACY_VALUE',
'Maximum model space distance between geometric entities at asserted c
onnectivities');
#12944=UNCERTAINTY_MEASURE_WITH_UNIT(LENGTH_MEASURE(0.001),#12964,
'DISTANCE_ACCURACY_VALUE',
'Maximum model space distance between geometric entities at asserted c
onnectivities');
#12945=UNCERTAINTY_MEASURE_WITH_UNIT(LENGTH_MEASURE(0.001),#12964,
'DISTANCE_ACCURACY_VALUE',
'Maximum model space distance between geometric entities at asserted c
onnectivities');
#12946=UNCERTAINTY_MEASURE_WITH_UNIT(LENGTH_MEASURE(0.001),#12964,
'DISTANCE_ACCURACY_VALUE',
'Maximum model space distance between geometric entities at asserted c
onnectivities');
#12947=UNCERTAINTY_MEASURE_WITH_UNIT(LENGTH_MEASURE(0.001),#12964,
'DISTANCE_ACCURACY_VALUE',
'Maximum model space distance between geometric entities at asserted c
onnectivities');
#12948=UNCERTAINTY_MEASURE_WITH_UNIT(LENGTH_MEASURE(0.001),#12964,
'DISTANCE_ACCURACY_VALUE',
'Maximum model space distance between geometric entities at asserted c
onnectivities');
#12949=UNCERTAINTY_MEASURE_WITH_UNIT(LENGTH_MEASURE(0.001),#12964,
'DISTANCE_ACCURACY_VALUE',
'Maximum model space distance between geometric entities at asserted c
onnectivities');
#12950=(
GEOMETRIC_REPRESENTATION_CONTEXT(3)
GLOBAL_UNCERTAINTY_ASSIGNED_CONTEXT((#12936))
GLOBAL_UNIT_ASSIGNED_CONTEXT((#12964,#12966,#12967))
REPRESENTATION_CONTEXT('','3D')
);
#12951=(
GEOMETRIC_REPRESENTATION_CONTEXT(3)
GLOBAL_UNCERTAINTY_ASSIGNED_CONTEXT((#12937))
GLOBAL_UNIT_ASSIGNED_CONTEXT((#12964,#12966,#12967))
REPRESENTATION_CONTEXT('','3D')
);
#12952=(
GEOMETRIC_REPRESENTATION_CONTEXT(3)
GLOBAL_UNCERTAINTY_ASSIGNED_CONTEXT((#12938))
GLOBAL_UNIT_ASSIGNED_CONTEXT((#12964,#12966,#12967))
REPRESENTATION_CONTEXT('','3D')
);
#12953=(
GEOMETRIC_REPRESENTATION_CONTEXT(3)
GLOBAL_UNCERTAINTY_ASSIGNED_CONTEXT((#12939))
GLOBAL_UNIT_ASSIGNED_CONTEXT((#12964,#12966,#12967))
REPRESENTATION_CONTEXT('','3D')
);
#12954=(
GEOMETRIC_REPRESENTATION_CONTEXT(3)
GLOBAL_UNCERTAINTY_ASSIGNED_CONTEXT((#12940))
GLOBAL_UNIT_ASSIGNED_CONTEXT((#12964,#12966,#12967))
REPRESENTATION_CONTEXT('','3D')
);
#12955=(
GEOMETRIC_REPRESENTATION_CONTEXT(3)
GLOBAL_UNCERTAINTY_ASSIGNED_CONTEXT((#12941))
GLOBAL_UNIT_ASSIGNED_CONTEXT((#12964,#12966,#12967))
REPRESENTATION_CONTEXT('','3D')
);
#12956=(
GEOMETRIC_REPRESENTATION_CONTEXT(3)
GLOBAL_UNCERTAINTY_ASSIGNED_CONTEXT((#12942))
GLOBAL_UNIT_ASSIGNED_CONTEXT((#12964,#12966,#12967))
REPRESENTATION_CONTEXT('','3D')
);
#12957=(
GEOMETRIC_REPRESENTATION_CONTEXT(3)
GLOBAL_UNCERTAINTY_ASSIGNED_CONTEXT((#12943))
GLOBAL_UNIT_ASSIGNED_CONTEXT((#12964,#12966,#12967))
REPRESENTATION_CONTEXT('','3D')
);
#12958=(
GEOMETRIC_REPRESENTATION_CONTEXT(3)
GLOBAL_UNCERTAINTY_ASSIGNED_CONTEXT((#12944))
GLOBAL_UNIT_ASSIGNED_CONTEXT((#12964,#12966,#12967))
REPRESENTATION_CONTEXT('','3D')
);
#12959=(
GEOMETRIC_REPRESENTATION_CONTEXT(3)
GLOBAL_UNCERTAINTY_ASSIGNED_CONTEXT((#12945))
GLOBAL_UNIT_ASSIGNED_CONTEXT((#12964,#12966,#12967))
REPRESENTATION_CONTEXT('','3D')
);
#12960=(
GEOMETRIC_REPRESENTATION_CONTEXT(3)
GLOBAL_UNCERTAINTY_ASSIGNED_CONTEXT((#12946))
GLOBAL_UNIT_ASSIGNED_CONTEXT((#12964,#12966,#12967))
REPRESENTATION_CONTEXT('','3D')
);
#12961=(
GEOMETRIC_REPRESENTATION_CONTEXT(3)
GLOBAL_UNCERTAINTY_ASSIGNED_CONTEXT((#12947))
GLOBAL_UNIT_ASSIGNED_CONTEXT((#12964,#12966,#12967))
REPRESENTATION_CONTEXT('','3D')
);
#12962=(
GEOMETRIC_REPRESENTATION_CONTEXT(3)
GLOBAL_UNCERTAINTY_ASSIGNED_CONTEXT((#12948))
GLOBAL_UNIT_ASSIGNED_CONTEXT((#12964,#12966,#12967))
REPRESENTATION_CONTEXT('','3D')
);
#12963=(
GEOMETRIC_REPRESENTATION_CONTEXT(3)
GLOBAL_UNCERTAINTY_ASSIGNED_CONTEXT((#12949))
GLOBAL_UNIT_ASSIGNED_CONTEXT((#12964,#12966,#12967))
REPRESENTATION_CONTEXT('','3D')
);
#12964=(
LENGTH_UNIT()
NAMED_UNIT(*)
SI_UNIT(.CENTI.,.METRE.)
);
#12965=(
LENGTH_UNIT()
NAMED_UNIT(*)
SI_UNIT($,.METRE.)
);
#12966=(
NAMED_UNIT(*)
PLANE_ANGLE_UNIT()
SI_UNIT($,.RADIAN.)
);
#12967=(
NAMED_UNIT(*)
SI_UNIT($,.STERADIAN.)
SOLID_ANGLE_UNIT()
);
#12968=SHAPE_DEFINITION_REPRESENTATION(#12981,#13034);
#12969=SHAPE_DEFINITION_REPRESENTATION(#12982,#13035);
#12970=SHAPE_DEFINITION_REPRESENTATION(#12983,#13036);
#12971=SHAPE_DEFINITION_REPRESENTATION(#12984,#13037);
#12972=SHAPE_DEFINITION_REPRESENTATION(#12985,#13038);
#12973=SHAPE_DEFINITION_REPRESENTATION(#12986,#13039);
#12974=SHAPE_DEFINITION_REPRESENTATION(#12987,#13040);
#12975=SHAPE_DEFINITION_REPRESENTATION(#12988,#13041);
#12976=SHAPE_DEFINITION_REPRESENTATION(#12989,#13042);
#12977=SHAPE_DEFINITION_REPRESENTATION(#12990,#13043);
#12978=SHAPE_DEFINITION_REPRESENTATION(#12991,#13044);
#12979=SHAPE_DEFINITION_REPRESENTATION(#12992,#13045);
#12980=SHAPE_DEFINITION_REPRESENTATION(#12993,#13046);
#12981=PRODUCT_DEFINITION_SHAPE('',$,#13048);
#12982=PRODUCT_DEFINITION_SHAPE('',$,#13049);
#12983=PRODUCT_DEFINITION_SHAPE('',$,#13050);
#12984=PRODUCT_DEFINITION_SHAPE('',$,#13051);
#12985=PRODUCT_DEFINITION_SHAPE('',$,#13052);
#12986=PRODUCT_DEFINITION_SHAPE('',$,#13053);
#12987=PRODUCT_DEFINITION_SHAPE('',$,#13054);
#12988=PRODUCT_DEFINITION_SHAPE('',$,#13055);
#12989=PRODUCT_DEFINITION_SHAPE('',$,#13056);
#12990=PRODUCT_DEFINITION_SHAPE('',$,#13057);
#12991=PRODUCT_DEFINITION_SHAPE('',$,#13058);
#12992=PRODUCT_DEFINITION_SHAPE('',$,#13059);
#12993=PRODUCT_DEFINITION_SHAPE('',$,#13060);
#12994=PRODUCT_DEFINITION_SHAPE($,$,#131);
#12995=PRODUCT_DEFINITION_SHAPE($,$,#132);
#12996=PRODUCT_DEFINITION_SHAPE($,$,#133);
#12997=PRODUCT_DEFINITION_SHAPE($,$,#134);
#12998=PRODUCT_DEFINITION_SHAPE($,$,#135);
#12999=PRODUCT_DEFINITION_SHAPE($,$,#136);
#13000=PRODUCT_DEFINITION_SHAPE($,$,#137);
#13001=PRODUCT_DEFINITION_SHAPE($,$,#138);
#13002=PRODUCT_DEFINITION_SHAPE($,$,#139);
#13003=PRODUCT_DEFINITION_SHAPE($,$,#140);
#13004=PRODUCT_DEFINITION_SHAPE($,$,#141);
#13005=PRODUCT_DEFINITION_SHAPE($,$,#142);
#13006=PRODUCT_DEFINITION_SHAPE($,$,#143);
#13007=PRODUCT_DEFINITION_SHAPE($,$,#144);
#13008=PRODUCT_DEFINITION_SHAPE($,$,#145);
#13009=PRODUCT_DEFINITION_SHAPE($,$,#146);
#13010=PRODUCT_DEFINITION_SHAPE($,$,#147);
#13011=PRODUCT_DEFINITION_SHAPE($,$,#148);
#13012=PRODUCT_DEFINITION_SHAPE($,$,#149);
#13013=PRODUCT_DEFINITION_SHAPE($,$,#150);
#13014=PRODUCT_DEFINITION_SHAPE($,$,#151);
#13015=PRODUCT_DEFINITION_SHAPE($,$,#152);
#13016=PRODUCT_DEFINITION_SHAPE($,$,#153);
#13017=PRODUCT_DEFINITION_SHAPE($,$,#154);
#13018=PRODUCT_DEFINITION_SHAPE($,$,#155);
#13019=PRODUCT_DEFINITION_SHAPE($,$,#156);
#13020=PRODUCT_DEFINITION_SHAPE($,$,#157);
#13021=PRODUCT_DEFINITION_SHAPE($,$,#158);
#13022=PRODUCT_DEFINITION_SHAPE($,$,#159);
#13023=PRODUCT_DEFINITION_SHAPE($,$,#160);
#13024=PRODUCT_DEFINITION_SHAPE($,$,#161);
#13025=PRODUCT_DEFINITION_SHAPE($,$,#162);
#13026=PRODUCT_DEFINITION_SHAPE($,$,#163);
#13027=PRODUCT_DEFINITION_SHAPE($,$,#164);
#13028=PRODUCT_DEFINITION_SHAPE($,$,#165);
#13029=PRODUCT_DEFINITION_SHAPE($,$,#166);
#13030=PRODUCT_DEFINITION_SHAPE($,$,#167);
#13031=PRODUCT_DEFINITION_SHAPE($,$,#168);
#13032=PRODUCT_DEFINITION_SHAPE($,$,#169);
#13033=PRODUCT_DEFINITION_SHAPE($,$,#170);
#13034=SHAPE_REPRESENTATION('',(#4954,#5301,#5302,#5303,#5304,#5305,#5306,
#5307,#5308,#5309,#5310,#5311,#5312,#5313,#5314,#5315,#5316,#5317,#5318,
#5319,#5320,#5321,#5322,#5323,#5324,#5325,#5326,#5327,#5328,#5329,#5330,
#5331,#5332,#5333,#5334,#5335,#5336,#5337,#5338,#5339,#5340),#12950);
#13035=SHAPE_REPRESENTATION('',(#4955),#12951);
#13036=SHAPE_REPRESENTATION('',(#5008),#12952);
#13037=SHAPE_REPRESENTATION('',(#5053),#12953);
#13038=SHAPE_REPRESENTATION('',(#5064),#12954);
#13039=SHAPE_REPRESENTATION('',(#5071),#12955);
#13040=SHAPE_REPRESENTATION('',(#5080),#12956);
#13041=SHAPE_REPRESENTATION('',(#5101),#12957);
#13042=SHAPE_REPRESENTATION('',(#5134),#12958);
#13043=SHAPE_REPRESENTATION('',(#5163),#12959);
#13044=SHAPE_REPRESENTATION('',(#5177),#12960);
#13045=SHAPE_REPRESENTATION('',(#5267),#12961);
#13046=SHAPE_REPRESENTATION('',(#5295),#12962);
#13047=PRODUCT_DEFINITION_CONTEXT('part definition',#13088,'design');
#13048=PRODUCT_DEFINITION('TAS-020','TAS-020',#13061,#13047);
#13049=PRODUCT_DEFINITION('Side panel with hardware clearance',
'Side panel with hardware clearance',#13062,#13047);
#13050=PRODUCT_DEFINITION('Universal side panel','Universal side panel',
#13063,#13047);
#13051=PRODUCT_DEFINITION('Horizontal closure panel',
'Horizontal closure panel',#13064,#13047);
#13052=PRODUCT_DEFINITION('Captured back panel','Captured back panel',#13065,
#13047);
#13053=PRODUCT_DEFINITION('Fixed shelf','Fixed shelf',#13066,#13047);
#13054=PRODUCT_DEFINITION('Door panel','Door panel',#13067,#13047);
#13055=PRODUCT_DEFINITION('Fabricated case hinge leaf',
'Fabricated case hinge leaf',#13068,#13047);
#13056=PRODUCT_DEFINITION('Fabricated door hinge leaf',
'Fabricated door hinge leaf',#13069,#13047);
#13057=PRODUCT_DEFINITION('Retained hinge pin','Retained hinge pin',#13070,
#13047);
#13058=PRODUCT_DEFINITION('Socket head screw M4x24',
'Socket head screw M4x24',#13071,#13047);
#13059=PRODUCT_DEFINITION('Hex nut M4','Hex nut M4',#13072,#13047);
#13060=PRODUCT_DEFINITION('Bay coupling dowel','Bay coupling dowel',#13073,
#13047);
#13061=PRODUCT_DEFINITION_FORMATION('',$,#13090);
#13062=PRODUCT_DEFINITION_FORMATION('',$,#13091);
#13063=PRODUCT_DEFINITION_FORMATION('',$,#13092);
#13064=PRODUCT_DEFINITION_FORMATION('',$,#13093);
#13065=PRODUCT_DEFINITION_FORMATION('',$,#13094);
#13066=PRODUCT_DEFINITION_FORMATION('',$,#13095);
#13067=PRODUCT_DEFINITION_FORMATION('',$,#13096);
#13068=PRODUCT_DEFINITION_FORMATION('',$,#13097);
#13069=PRODUCT_DEFINITION_FORMATION('',$,#13098);
#13070=PRODUCT_DEFINITION_FORMATION('',$,#13099);
#13071=PRODUCT_DEFINITION_FORMATION('',$,#13100);
#13072=PRODUCT_DEFINITION_FORMATION('',$,#13101);
#13073=PRODUCT_DEFINITION_FORMATION('',$,#13102);
#13074=PRODUCT_RELATED_PRODUCT_CATEGORY('TAS-020','TAS-020',(#13090));
#13075=PRODUCT_RELATED_PRODUCT_CATEGORY(
'Side panel with hardware clearance',
'Side panel with hardware clearance',(#13091));
#13076=PRODUCT_RELATED_PRODUCT_CATEGORY('Universal side panel',
'Universal side panel',(#13092));
#13077=PRODUCT_RELATED_PRODUCT_CATEGORY('Horizontal closure panel',
'Horizontal closure panel',(#13093));
#13078=PRODUCT_RELATED_PRODUCT_CATEGORY('Captured back panel',
'Captured back panel',(#13094));
#13079=PRODUCT_RELATED_PRODUCT_CATEGORY('Fixed shelf','Fixed shelf',(#13095));
#13080=PRODUCT_RELATED_PRODUCT_CATEGORY('Door panel','Door panel',(#13096));
#13081=PRODUCT_RELATED_PRODUCT_CATEGORY('Fabricated case hinge leaf',
'Fabricated case hinge leaf',(#13097));
#13082=PRODUCT_RELATED_PRODUCT_CATEGORY('Fabricated door hinge leaf',
'Fabricated door hinge leaf',(#13098));
#13083=PRODUCT_RELATED_PRODUCT_CATEGORY('Retained hinge pin',
'Retained hinge pin',(#13099));
#13084=PRODUCT_RELATED_PRODUCT_CATEGORY('Socket head screw M4x24',
'Socket head screw M4x24',(#13100));
#13085=PRODUCT_RELATED_PRODUCT_CATEGORY('Hex nut M4','Hex nut M4',(#13101));
#13086=PRODUCT_RELATED_PRODUCT_CATEGORY('Bay coupling dowel',
'Bay coupling dowel',(#13102));
#13087=APPLICATION_PROTOCOL_DEFINITION('international standard',
'automotive_design',2009,#13088);
#13088=APPLICATION_CONTEXT(
'Core Data for Automotive Mechanical Design Process');
#13089=PRODUCT_CONTEXT('part definition',#13088,'mechanical');
#13090=PRODUCT('TAS-020','TAS-020',$,(#13089));
#13091=PRODUCT('Side panel with hardware clearance',
'Side panel with hardware clearance',$,(#13089));
#13092=PRODUCT('Universal side panel','Universal side panel',$,(#13089));
#13093=PRODUCT('Horizontal closure panel','Horizontal closure panel',$,
(#13089));
#13094=PRODUCT('Captured back panel','Captured back panel',$,(#13089));
#13095=PRODUCT('Fixed shelf','Fixed shelf',$,(#13089));
#13096=PRODUCT('Door panel','Door panel','Door panel',(#13089));
#13097=PRODUCT('Fabricated case hinge leaf',
'Fabricated case hinge leaf',$,(#13089));
#13098=PRODUCT('Fabricated door hinge leaf',
'Fabricated door hinge leaf',$,(#13089));
#13099=PRODUCT('Retained hinge pin','Retained hinge pin',$,(#13089));
#13100=PRODUCT('Socket head screw M4x24','Socket head screw M4x24',$,(#13089));
#13101=PRODUCT('Hex nut M4','Hex nut M4',$,(#13089));
#13102=PRODUCT('Bay coupling dowel','Bay coupling dowel',$,(#13089));
#13103=PRESENTATION_STYLE_ASSIGNMENT((#13116));
#13104=PRESENTATION_STYLE_ASSIGNMENT((#13117));
#13105=PRESENTATION_STYLE_ASSIGNMENT((#13118));
#13106=PRESENTATION_STYLE_ASSIGNMENT((#13119));
#13107=PRESENTATION_STYLE_ASSIGNMENT((#13120));
#13108=PRESENTATION_STYLE_ASSIGNMENT((#13121));
#13109=PRESENTATION_STYLE_ASSIGNMENT((#13122));
#13110=PRESENTATION_STYLE_ASSIGNMENT((#13123));
#13111=PRESENTATION_STYLE_ASSIGNMENT((#13124));
#13112=PRESENTATION_STYLE_ASSIGNMENT((#13125));
#13113=PRESENTATION_STYLE_ASSIGNMENT((#13126));
#13114=PRESENTATION_STYLE_ASSIGNMENT((#13127));
#13115=PRESENTATION_STYLE_ASSIGNMENT((#13128));
#13116=SURFACE_STYLE_USAGE(.BOTH.,#13129);
#13117=SURFACE_STYLE_USAGE(.BOTH.,#13130);
#13118=SURFACE_STYLE_USAGE(.BOTH.,#13131);
#13119=SURFACE_STYLE_USAGE(.BOTH.,#13132);
#13120=SURFACE_STYLE_USAGE(.BOTH.,#13133);
#13121=SURFACE_STYLE_USAGE(.BOTH.,#13134);
#13122=SURFACE_STYLE_USAGE(.BOTH.,#13135);
#13123=SURFACE_STYLE_USAGE(.BOTH.,#13136);
#13124=SURFACE_STYLE_USAGE(.BOTH.,#13137);
#13125=SURFACE_STYLE_USAGE(.BOTH.,#13138);
#13126=SURFACE_STYLE_USAGE(.BOTH.,#13139);
#13127=SURFACE_STYLE_USAGE(.BOTH.,#13140);
#13128=SURFACE_STYLE_USAGE(.BOTH.,#13141);
#13129=SURFACE_SIDE_STYLE('',(#13142));
#13130=SURFACE_SIDE_STYLE('',(#13143));
#13131=SURFACE_SIDE_STYLE('',(#13144));
#13132=SURFACE_SIDE_STYLE('',(#13145));
#13133=SURFACE_SIDE_STYLE('',(#13146));
#13134=SURFACE_SIDE_STYLE('',(#13147));
#13135=SURFACE_SIDE_STYLE('',(#13148));
#13136=SURFACE_SIDE_STYLE('',(#13149));
#13137=SURFACE_SIDE_STYLE('',(#13150));
#13138=SURFACE_SIDE_STYLE('',(#13151));
#13139=SURFACE_SIDE_STYLE('',(#13152));
#13140=SURFACE_SIDE_STYLE('',(#13153));
#13141=SURFACE_SIDE_STYLE('',(#13154));
#13142=SURFACE_STYLE_FILL_AREA(#13155);
#13143=SURFACE_STYLE_FILL_AREA(#13156);
#13144=SURFACE_STYLE_FILL_AREA(#13157);
#13145=SURFACE_STYLE_FILL_AREA(#13158);
#13146=SURFACE_STYLE_FILL_AREA(#13159);
#13147=SURFACE_STYLE_FILL_AREA(#13160);
#13148=SURFACE_STYLE_FILL_AREA(#13161);
#13149=SURFACE_STYLE_FILL_AREA(#13162);
#13150=SURFACE_STYLE_FILL_AREA(#13163);
#13151=SURFACE_STYLE_FILL_AREA(#13164);
#13152=SURFACE_STYLE_FILL_AREA(#13165);
#13153=SURFACE_STYLE_FILL_AREA(#13166);
#13154=SURFACE_STYLE_FILL_AREA(#13167);
#13155=FILL_AREA_STYLE('Steel - Satin',(#13168));
#13156=FILL_AREA_STYLE('Side panel with hardware clearance finish',(#13169));
#13157=FILL_AREA_STYLE('Universal side panel finish',(#13170));
#13158=FILL_AREA_STYLE('Horizontal closure panel finish',(#13171));
#13159=FILL_AREA_STYLE('Captured back panel finish',(#13172));
#13160=FILL_AREA_STYLE('Fixed shelf finish',(#13173));
#13161=FILL_AREA_STYLE('Door panel finish',(#13174));
#13162=FILL_AREA_STYLE('Fabricated case hinge leaf finish',(#13175));
#13163=FILL_AREA_STYLE('Fabricated door hinge leaf finish',(#13176));
#13164=FILL_AREA_STYLE('Retained hinge pin finish',(#13177));
#13165=FILL_AREA_STYLE('Socket head screw M4x24 finish',(#13178));
#13166=FILL_AREA_STYLE('Hex nut M4 finish',(#13179));
#13167=FILL_AREA_STYLE('Bay coupling dowel finish',(#13180));
#13168=FILL_AREA_STYLE_COLOUR('Steel - Satin',#13181);
#13169=FILL_AREA_STYLE_COLOUR(
'Side panel with hardware clearance finish',#13182);
#13170=FILL_AREA_STYLE_COLOUR('Universal side panel finish',#13183);
#13171=FILL_AREA_STYLE_COLOUR('Horizontal closure panel finish',#13184);
#13172=FILL_AREA_STYLE_COLOUR('Captured back panel finish',#13185);
#13173=FILL_AREA_STYLE_COLOUR('Fixed shelf finish',#13186);
#13174=FILL_AREA_STYLE_COLOUR('Door panel finish',#13187);
#13175=FILL_AREA_STYLE_COLOUR('Fabricated case hinge leaf finish',#13188);
#13176=FILL_AREA_STYLE_COLOUR('Fabricated door hinge leaf finish',#13189);
#13177=FILL_AREA_STYLE_COLOUR('Retained hinge pin finish',#13190);
#13178=FILL_AREA_STYLE_COLOUR('Socket head screw M4x24 finish',#13191);
#13179=FILL_AREA_STYLE_COLOUR('Hex nut M4 finish',#13192);
#13180=FILL_AREA_STYLE_COLOUR('Bay coupling dowel finish',#13193);
#13181=COLOUR_RGB('Steel - Satin',0.627450980392157,0.627450980392157,0.627450980392157);
#13182=COLOUR_RGB('Side panel with hardware clearance finish',0.0941176470588235,
0.231372549019608,0.431372549019608);
#13183=COLOUR_RGB('Universal side panel finish',0.0941176470588235,0.231372549019608,
0.431372549019608);
#13184=COLOUR_RGB('Horizontal closure panel finish',0.662745098039216,0.823529411764706,
0.917647058823529);
#13185=COLOUR_RGB('Captured back panel finish',0.607843137254902,0.647058823529412,
0.701960784313725);
#13186=COLOUR_RGB('Fixed shelf finish',0.274509803921569,0.6,0.8);
#13187=COLOUR_RGB('Door panel finish',0.274509803921569,0.6,0.8);
#13188=COLOUR_RGB('Fabricated case hinge leaf finish',0.607843137254902,
0.647058823529412,0.701960784313725);
#13189=COLOUR_RGB('Fabricated door hinge leaf finish',0.607843137254902,
0.647058823529412,0.701960784313725);
#13190=COLOUR_RGB('Retained hinge pin finish',0.294117647058824,0.317647058823529,
0.36078431372549);
#13191=COLOUR_RGB('Socket head screw M4x24 finish',0.607843137254902,0.647058823529412,
0.701960784313725);
#13192=COLOUR_RGB('Hex nut M4 finish',0.607843137254902,0.647058823529412,
0.701960784313725);
#13193=COLOUR_RGB('Bay coupling dowel finish',0.43921568627451,0.47843137254902,
0.52156862745098);
ENDSEC;
END-ISO-10303-21;
